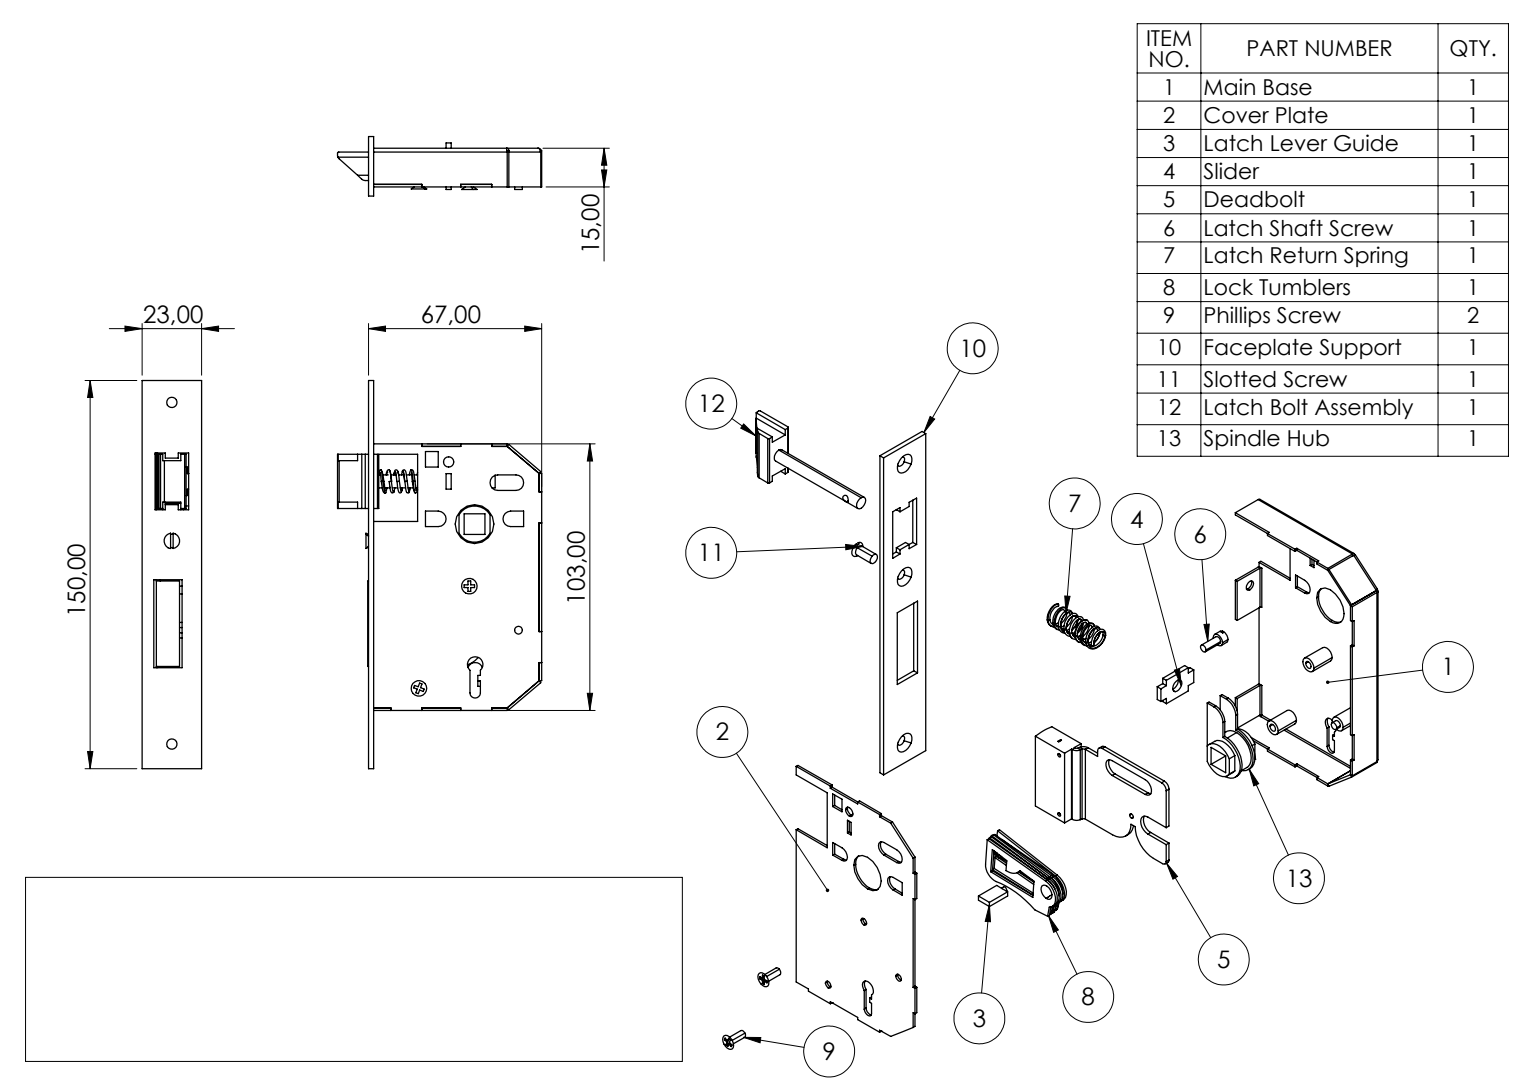
ISO-10303-21;
HEADER;
FILE_DESCRIPTION (('STEP AP214'),
    '1' );
FILE_NAME ('MAS-159',
    '2026-10-06T13:23:30',
    ( '' ),
    ( '' ),
    'SwSTEP 2.0',
    'SolidWorks 2020',
    '' );
FILE_SCHEMA (( 'AUTOMOTIVE_DESIGN' ));
ENDSEC;

DATA;
#1 = VERTEX_POINT ( 'NONE', #187 ) ;
#2 = FACE_OUTER_BOUND ( 'NONE', #19323, .T. ) ;
#3 = VECTOR ( 'NONE', #8048, 1000.000000000000000 ) ;
#4 = CARTESIAN_POINT ( 'NONE',  ( -30.49999999990000177, 47.50000000000000000, -147.5552959529999839 ) ) ;
#5 = CARTESIAN_POINT ( 'NONE',  ( -17.23399296970191941, 39.75881394383647915, -140.1956667236787553 ) ) ;
#6 = CARTESIAN_POINT ( 'NONE',  ( -31.50000000000000000, 10.25000000000000000, -137.0552959530000123 ) ) ;
#7 = ORIENTED_EDGE ( 'NONE', *, *, #14186, .F. ) ;
#8 = PLANE ( 'NONE',  #9401 ) ;
#9 = LINE ( 'NONE', #19761, #1381 ) ;
#10 = VECTOR ( 'NONE', #7060, 1000.000000000000000 ) ;
#11 = AXIS2_PLACEMENT_3D ( 'NONE', #8337, #8458, #15612 ) ;
#12 = LINE ( 'NONE', #7259, #31 ) ;
#13 = DIRECTION ( 'NONE',  ( 0.000000000000000000, 1.000000000000000000, 0.000000000000000000 ) ) ;
#14 = CARTESIAN_POINT ( 'NONE',  ( 7.750000000000000000, -40.23606797749999942, -150.0552959529999839 ) ) ;
#15 = VECTOR ( 'NONE', #22356, 1000.000000000000000 ) ;
#16 = CARTESIAN_POINT ( 'NONE',  ( -31.00000000000000000, 10.25000000000000000, -150.0552959529999839 ) ) ;
#17 = VECTOR ( 'NONE', #19861, 1000.000000000000114 ) ;
#18 = ORIENTED_EDGE ( 'NONE', *, *, #14112, .F. ) ;
#19 = EDGE_CURVE ( 'NONE', #10851, #14365, #21344, .T. ) ;
#20 = LINE ( 'NONE', #12366, #11445 ) ;
#21 = CARTESIAN_POINT ( 'NONE',  ( -13.53805010459570823, -42.60941606008491789, -136.0552959529695158 ) ) ;
#22 = EDGE_CURVE ( 'NONE', #8505, #15326, #21385, .T. ) ;
#23 = CARTESIAN_POINT ( 'NONE',  ( 6.899000527194547594, -5.343640159924734512, -150.0552959529999839 ) ) ;
#24 = CARTESIAN_POINT ( 'NONE',  ( -5.972224716186543603, 40.79464204718496489, -141.7656025440738006 ) ) ;
#25 = EDGE_CURVE ( 'NONE', #1116, #6470, #1636, .T. ) ;
#26 = CARTESIAN_POINT ( 'NONE',  ( 32.14594224149999491, 40.79958733410000349, -149.5552959519999945 ) ) ;
#27 = EDGE_LOOP ( 'NONE', ( #14113, #8328, #12180, #9090 ) ) ;
#28 = LINE ( 'NONE', #12848, #13253 ) ;
#29 = DIRECTION ( 'NONE',  ( -2.842170943040000002E-14, -3.552713678800000097E-13, -1.000000000000000000 ) ) ;
#30 = VERTEX_POINT ( 'NONE', #23278 ) ;
#31 = VECTOR ( 'NONE', #17982, 1000.000000000000000 ) ;
#32 = VECTOR ( 'NONE', #119, 1000.000000000000000 ) ;
#33 = DIRECTION ( 'NONE',  ( -2.257144641399999941E-12, 0.000000000000000000, -1.000000000000000000 ) ) ;
#34 = VERTEX_POINT ( 'NONE', #8858 ) ;
#35 = FACE_OUTER_BOUND ( 'NONE', #21489, .T. ) ;
#36 = CARTESIAN_POINT ( 'NONE',  ( -30.18072937777062492, 41.58839647259347316, -144.3146225325547505 ) ) ;
#37 = CARTESIAN_POINT ( 'NONE',  ( 5.631397321050000571, -17.85059010000000157, -146.5552959529999839 ) ) ;
#38 = CARTESIAN_POINT ( 'NONE',  ( 7.263251615191055777, 37.84880977052021223, -141.7037997430943790 ) ) ;
#39 = ORIENTED_EDGE ( 'NONE', *, *, #18140, .F. ) ;
#40 = CARTESIAN_POINT ( 'NONE',  ( -11.30159772195502299, 34.40649072814353815, -140.3533750429825773 ) ) ;
#41 = CARTESIAN_POINT ( 'NONE',  ( -19.36238656785138090, 32.32519816855536732, -144.8017779651653427 ) ) ;
#42 = DIRECTION ( 'NONE',  ( 0.000000000000000000, 1.000000000000000000, 0.000000000000000000 ) ) ;
#43 = DIRECTION ( 'NONE',  ( 0.000000000000000000, 1.000000000000000000, 0.000000000000000000 ) ) ;
#44 = ORIENTED_EDGE ( 'NONE', *, *, #15140, .T. ) ;
#45 = VECTOR ( 'NONE', #10247, 1000.000000000000000 ) ;
#46 = CARTESIAN_POINT ( 'NONE',  ( -26.35824191589999899, -34.50000000000000000, -150.0657682190000060 ) ) ;
#47 = ORIENTED_EDGE ( 'NONE', *, *, #19254, .F. ) ;
#48 = CARTESIAN_POINT ( 'NONE',  ( -8.100541861814468447, 36.99062475582145737, -140.7379126119401178 ) ) ;
#49 = DIRECTION ( 'NONE',  ( -2.507771768020000122E-12, -0.000000000000000000, 1.000000000000000000 ) ) ;
#50 = EDGE_CURVE ( 'NONE', #22537, #320, #23237, .T. ) ;
#51 = CARTESIAN_POINT ( 'NONE',  ( 23.00000000000000000, 25.50000000000000000, -151.0552959529999839 ) ) ;
#52 = ORIENTED_EDGE ( 'NONE', *, *, #9220, .T. ) ;
#53 = DIRECTION ( 'NONE',  ( 1.000000000000000000, 0.000000000000000000, 0.000000000000000000 ) ) ;
#54 = LINE ( 'NONE', #14445, #10 ) ;
#55 = ORIENTED_EDGE ( 'NONE', *, *, #18140, .T. ) ;
#56 = CARTESIAN_POINT ( 'NONE',  ( -17.71126569040000120, 40.30718541979999969, -145.9389846960000057 ) ) ;
#57 = EDGE_CURVE ( 'NONE', #16606, #2360, #10514, .T. ) ;
#58 = CARTESIAN_POINT ( 'NONE',  ( 18.66060904160396916, 20.09818317339116689, -150.0552959529999839 ) ) ;
#59 = CARTESIAN_POINT ( 'NONE',  ( -15.75723547076485254, -44.30951848884578226, -150.0552959529999839 ) ) ;
#60 = AXIS2_PLACEMENT_3D ( 'NONE', #23173, #12444, #1408 ) ;
#61 = CLOSED_SHELL ( 'NONE', ( #2527, #3162, #21913, #12259, #23509, #6478, #21323, #18404, #11266, #1129, #5411, #9358, #21072, #12421, #16618, #19421, #14593, #11107, #12865, #16221, #14697, #10087, #8870, #20532, #21101, #11720, #17202, #7335, #11973, #7291, #21318, #13553, #10889, #7699, #12447, #10834 ) ) ;
#62 = FACE_OUTER_BOUND ( 'NONE', #19920, .T. ) ;
#63 = VECTOR ( 'NONE', #17679, 1000.000000000000000 ) ;
#64 = LINE ( 'NONE', #5521, #16191 ) ;
#65 = LINE ( 'NONE', #14804, #22679 ) ;
#66 = PLANE ( 'NONE',  #21173 ) ;
#67 = CARTESIAN_POINT ( 'NONE',  ( 15.97954986339999905, -26.72957102550000030, -142.5552959529999839 ) ) ;
#68 = EDGE_CURVE ( 'NONE', #3612, #21024, #1516, .T. ) ;
#69 = CARTESIAN_POINT ( 'NONE',  ( -4.946601369560000627, -23.77962690289999870, -143.5552959529999839 ) ) ;
#70 = VERTEX_POINT ( 'NONE', #16012 ) ;
#71 = ORIENTED_EDGE ( 'NONE', *, *, #16428, .T. ) ;
#72 =( NAMED_UNIT ( * ) PLANE_ANGLE_UNIT ( ) SI_UNIT ( $, .RADIAN. ) );
#73 = VERTEX_POINT ( 'NONE', #5299 ) ;
#74 = FACE_OUTER_BOUND ( 'NONE', #19510, .T. ) ;
#75 = CARTESIAN_POINT ( 'NONE',  ( 7.750000000000000000, -40.23606797749999942, -150.5552959529999839 ) ) ;
#76 = VERTEX_POINT ( 'NONE', #12547 ) ;
#77 = AXIS2_PLACEMENT_3D ( 'NONE', #19282, #2992, #15716 ) ;
#78 = EDGE_CURVE ( 'NONE', #537, #6609, #18037, .T. ) ;
#79 = CIRCLE ( 'NONE', #13356, 2.000000000000000000 ) ;
#80 = CARTESIAN_POINT ( 'NONE',  ( 1.600095057559999923, -18.40127899619999852, -146.5552959529999839 ) ) ;
#81 = VECTOR ( 'NONE', #14435, 1000.000000000000114 ) ;
#82 = ORIENTED_EDGE ( 'NONE', *, *, #12596, .T. ) ;
#83 = CARTESIAN_POINT ( 'NONE',  ( 6.499999999879999102, -3.000000000000000000, -135.2552959529999725 ) ) ;
#84 = CARTESIAN_POINT ( 'NONE',  ( -19.91646121121569735, 34.85517757522313076, -141.3256718703773629 ) ) ;
#85 = CARTESIAN_POINT ( 'NONE',  ( -30.02199999990000023, 40.03108891319999429, -145.8052959529999839 ) ) ;
#86 = CARTESIAN_POINT ( 'NONE',  ( 15.50000000000000000, 39.50000000000000000, -136.0552959530000123 ) ) ;
#87 = ORIENTED_EDGE ( 'NONE', *, *, #14036, .T. ) ;
#88 = DIRECTION ( 'NONE',  ( 2.257749542879999954E-12, 0.000000000000000000, 1.000000000000000000 ) ) ;
#89 = ORIENTED_EDGE ( 'NONE', *, *, #22160, .F. ) ;
#90 = EDGE_CURVE ( 'NONE', #4045, #3279, #299, .T. ) ;
#91 = CARTESIAN_POINT ( 'NONE',  ( 9.327001754561790037, 35.74856537270147783, -141.8910607813375009 ) ) ;
#92 = DIRECTION ( 'NONE',  ( -2.257144641399999941E-12, 8.049635416090000264E-35, -1.000000000000000000 ) ) ;
#93 = DIRECTION ( 'NONE',  ( -0.9892101392001054760, 0.1465035852930155480, 4.471739159800472250E-12 ) ) ;
#94 = VECTOR ( 'NONE', #6253, 1000.000000000000000 ) ;
#95 = ORIENTED_EDGE ( 'NONE', *, *, #4265, .F. ) ;
#96 = VECTOR ( 'NONE', #17767, 1000.000000000000227 ) ;
#97 = AXIS2_PLACEMENT_3D ( 'NONE', #8071, #2741, #23074 ) ;
#98 = EDGE_CURVE ( 'NONE', #6545, #18690, #5646, .T. ) ;
#99 = EDGE_CURVE ( 'NONE', #3836, #1507, #11570, .T. ) ;
#100 = PLANE ( 'NONE',  #11800 ) ;
#101 = ORIENTED_EDGE ( 'NONE', *, *, #18336, .T. ) ;
#102 = DIRECTION ( 'NONE',  ( 0.000000000000000000, -1.000000000000000000, 0.000000000000000000 ) ) ;
#103 = CARTESIAN_POINT ( 'NONE',  ( -6.024730888589999722, -51.50000000000000000, -149.5552959529999839 ) ) ;
#104 = EDGE_CURVE ( 'NONE', #6667, #13256, #16589, .T. ) ;
#105 = ORIENTED_EDGE ( 'NONE', *, *, #1127, .F. ) ;
#106 = PLANE ( 'NONE',  #15659 ) ;
#107 = ORIENTED_EDGE ( 'NONE', *, *, #17048, .F. ) ;
#108 = CARTESIAN_POINT ( 'NONE',  ( -21.95493828276233472, 34.13232134794248651, -147.9325040407576353 ) ) ;
#109 = EDGE_CURVE ( 'NONE', #2866, #16847, #2210, .T. ) ;
#110 = CARTESIAN_POINT ( 'NONE',  ( -25.86630785129999666, -51.50000000000000000, -136.5552959530000123 ) ) ;
#111 = ORIENTED_EDGE ( 'NONE', *, *, #15327, .F. ) ;
#112 = APPLICATION_PROTOCOL_DEFINITION ( 'draft international standard', 'automotive_design', 1998, #2963 ) ;
#113 = ORIENTED_EDGE ( 'NONE', *, *, #15897, .T. ) ;
#114 = CARTESIAN_POINT ( 'NONE',  ( -26.86882954950000268, 40.29793777999999804, -142.0811670120000088 ) ) ;
#115 = FACE_OUTER_BOUND ( 'NONE', #19032, .T. ) ;
#116 = MECHANICAL_DESIGN_GEOMETRIC_PRESENTATION_REPRESENTATION (  '', ( #11103 ), #3517 ) ;
#117 = CARTESIAN_POINT ( 'NONE',  ( -4.959431410700000598, -23.66636161550000139, -146.0552959529999839 ) ) ;
#118 = AXIS2_PLACEMENT_3D ( 'NONE', #14379, #10436, #6880 ) ;
#119 = DIRECTION ( 'NONE',  ( -1.000000000000000000, 0.000000000000000000, 2.245315044999999693E-12 ) ) ;
#120 = LINE ( 'NONE', #16055, #20099 ) ;
#121 = ORIENTED_EDGE ( 'NONE', *, *, #3001, .T. ) ;
#122 = CARTESIAN_POINT ( 'NONE',  ( -4.160432423080000497, -28.71743394529999804, -144.5552959529999839 ) ) ;
#123 = CARTESIAN_POINT ( 'NONE',  ( 10.38320006080000013, -24.50000000000000000, -148.5552959529999839 ) ) ;
#124 = ORIENTED_EDGE ( 'NONE', *, *, #13380, .T. ) ;
#125 = LINE ( 'NONE', #11042, #20030 ) ;
#126 = DIRECTION ( 'NONE',  ( 0.000000000000000000, 0.000000000000000000, 1.000000000000000000 ) ) ;
#127 = EDGE_CURVE ( 'NONE', #16762, #17721, #6116, .T. ) ;
#128 = CARTESIAN_POINT ( 'NONE',  ( -17.11288009319332915, 40.89466944836319584, -143.6359263498834196 ) ) ;
#129 = DIRECTION ( 'NONE',  ( -0.9896415801065050477, 0.1435602414469278887, 8.992806499463764746E-12 ) ) ;
#130 = EDGE_LOOP ( 'NONE', ( #1409, #6613, #421, #6495 ) ) ;
#131 = FACE_OUTER_BOUND ( 'NONE', #19542, .T. ) ;
#132 = DIRECTION ( 'NONE',  ( 1.000000000000000000, 0.000000000000000000, 0.000000000000000000 ) ) ;
#133 = CARTESIAN_POINT ( 'NONE',  ( 5.631397321050000571, -17.85059010000000157, -146.5552959529999839 ) ) ;
#134 = LINE ( 'NONE', #14635, #4183 ) ;
#135 = DIRECTION ( 'NONE',  ( 1.000000000000000000, 2.602084704489999637E-17, 0.000000000000000000 ) ) ;
#136 = LINE ( 'NONE', #21434, #17431 ) ;
#137 = ORIENTED_EDGE ( 'NONE', *, *, #3234, .F. ) ;
#138 = DIRECTION ( 'NONE',  ( 1.000000000000000000, 0.000000000000000000, -2.257560236040000027E-12 ) ) ;
#139 = CARTESIAN_POINT ( 'NONE',  ( -26.35824191589999899, -34.50000000000000000, -141.0657682190000060 ) ) ;
#140 = CARTESIAN_POINT ( 'NONE',  ( -18.07392865170000107, -1.500000000000000000, -147.3157682190000060 ) ) ;
#141 = CARTESIAN_POINT ( 'NONE',  ( -7.010349702009219364, 37.05829245175948472, -148.1453878979395995 ) ) ;
#142 = CARTESIAN_POINT ( 'NONE',  ( -13.80049973640272931, -43.92182007996237303, -136.0552959530027124 ) ) ;
#143 = EDGE_LOOP ( 'NONE', ( #7087, #11554, #3660, #16017 ) ) ;
#144 = CARTESIAN_POINT ( 'NONE',  ( 9.683200060759999062, -20.50000000000000000, -149.3052959529999839 ) ) ;
#145 = FACE_BOUND ( 'NONE', #10019, .T. ) ;
#146 = AXIS2_PLACEMENT_3D ( 'NONE', #6998, #10782, #18066 ) ;
#147 = ORIENTED_EDGE ( 'NONE', *, *, #18826, .F. ) ;
#148 = ORIENTED_EDGE ( 'NONE', *, *, #4162, .F. ) ;
#149 = CARTESIAN_POINT ( 'NONE',  ( 5.420128080818026106, -2.298969449354696604, -136.0552959530122337 ) ) ;
#150 = EDGE_CURVE ( 'NONE', #19192, #2146, #2095, .T. ) ;
#151 = CARTESIAN_POINT ( 'NONE',  ( -29.72253042784264210, 40.43424528537140361, -140.6915255650335723 ) ) ;
#152 = PLANE ( 'NONE',  #286 ) ;
#153 = CARTESIAN_POINT ( 'NONE',  ( 8.154916571317706087, 35.54018629028437459, -142.0257885890718512 ) ) ;
#154 = VERTEX_POINT ( 'NONE', #4337 ) ;
#155 = CARTESIAN_POINT ( 'NONE',  ( -10.36638211085415584, 32.95473824138212393, -141.4495653476137704 ) ) ;
#156 = CARTESIAN_POINT ( 'NONE',  ( -18.21358191688009498, 34.41669922854067920, -147.7040578527177388 ) ) ;
#157 = DIRECTION ( 'NONE',  ( 0.000000000000000000, 1.000000000000000000, 0.000000000000000000 ) ) ;
#158 = CARTESIAN_POINT ( 'NONE',  ( 9.295843182404178506, -32.13416640351051967, -136.0552959530209876 ) ) ;
#159 = CARTESIAN_POINT ( 'NONE',  ( -22.66750349916592810, 37.99877533998466816, -139.6205617058595294 ) ) ;
#160 = LINE ( 'NONE', #11080, #6868 ) ;
#161 = AXIS2_PLACEMENT_3D ( 'NONE', #17240, #17123, #840 ) ;
#162 = FACE_OUTER_BOUND ( 'NONE', #18152, .T. ) ;
#163 = DIRECTION ( 'NONE',  ( -2.808280234689999718E-18, 1.000000000000000000, 1.592654863519999645E-17 ) ) ;
#164 = CARTESIAN_POINT ( 'NONE',  ( -9.056357402059999728, -12.43025388040000045, -147.5552959529999839 ) ) ;
#165 = ORIENTED_EDGE ( 'NONE', *, *, #16079, .F. ) ;
#166 = CARTESIAN_POINT ( 'NONE',  ( -5.932764524189999555, 37.76833845600000217, -147.9772051180000005 ) ) ;
#167 = EDGE_LOOP ( 'NONE', ( #4339, #16056, #21520, #10157 ) ) ;
#168 = LINE ( 'NONE', #11551, #791 ) ;
#169 = CARTESIAN_POINT ( 'NONE',  ( 32.50000000000000000, 40.03620104880000241, -143.0552959529999839 ) ) ;
#170 = DIRECTION ( 'NONE',  ( -0.7071067811865474617, -0.7071067811865476838, 0.000000000000000000 ) ) ;
#171 = CARTESIAN_POINT ( 'NONE',  ( -3.500000000000000000, 44.50000000000000000, -150.0552959529999839 ) ) ;
#172 = ADVANCED_FACE ( 'NONE', ( #21960 ), #4222, .F. ) ;
#173 = DIRECTION ( 'NONE',  ( -0.09606172499277214338, -0.9953753789357123738, 8.234154099303244678E-13 ) ) ;
#174 = VECTOR ( 'NONE', #17768, 1000.000000000000000 ) ;
#175 = CARTESIAN_POINT ( 'NONE',  ( -7.816799939239999162, -1.500000000000000000, -148.5552959529999839 ) ) ;
#176 = DIRECTION ( 'NONE',  ( 2.507771768019999718E-12, 1.592654864069999939E-17, -1.000000000000000000 ) ) ;
#177 = EDGE_CURVE ( 'NONE', #22553, #21627, #7661, .T. ) ;
#178 = CARTESIAN_POINT ( 'NONE',  ( -1.499999999960000219, 44.50000000000000000, -136.0552959530000123 ) ) ;
#179 = PRODUCT ( 'Latch Shaft Screw', 'Latch Shaft Screw', '', ( #7074 ) ) ;
#180 = CARTESIAN_POINT ( 'NONE',  ( -33.42928932190000069, 66.02782287919998794, -146.7500980969999773 ) ) ;
#181 = ORIENTED_EDGE ( 'NONE', *, *, #506, .F. ) ;
#182 = UNCERTAINTY_MEASURE_WITH_UNIT (LENGTH_MEASURE( 1.000000000000000082E-05 ), #19737, 'distance_accuracy_value', 'NONE');
#183 = EDGE_LOOP ( 'NONE', ( #12514, #3187, #13299, #6261 ) ) ;
#184 = EDGE_LOOP ( 'NONE', ( #18556, #23230 ) ) ;
#185 = CARTESIAN_POINT ( 'NONE',  ( -16.74070468267852618, 33.96681352825373779, -142.1712902011884978 ) ) ;
#186 = CARTESIAN_POINT ( 'NONE',  ( 31.50000000000000000, 39.80430157320000006, -149.5552959529999839 ) ) ;
#187 = CARTESIAN_POINT ( 'NONE',  ( -20.60824191591068555, -32.00000000000000000, -141.9623572383543717 ) ) ;
#188 = CARTESIAN_POINT ( 'NONE',  ( 31.00000000000000000, 39.80430157320000006, -150.0552959529999839 ) ) ;
#189 = ORIENTED_EDGE ( 'NONE', *, *, #7703, .T. ) ;
#190 = DIRECTION ( 'NONE',  ( -2.257039000139999987E-12, 0.000000000000000000, -1.000000000000000000 ) ) ;
#191 = CARTESIAN_POINT ( 'NONE',  ( -19.09494877074376262, 33.54410563133428269, -142.1858765932176141 ) ) ;
#192 = CARTESIAN_POINT ( 'NONE',  ( 31.50000000000000000, 36.50000000000000000, -137.0552959530000123 ) ) ;
#193 = ORIENTED_EDGE ( 'NONE', *, *, #5602, .T. ) ;
#194 = LINE ( 'NONE', #5434, #7982 ) ;
#195 = EDGE_CURVE ( 'NONE', #7827, #16530, #20002, .T. ) ;
#196 = CARTESIAN_POINT ( 'NONE',  ( -31.00000000000000000, -50.00000000000000000, -151.0552959529999839 ) ) ;
#197 = CARTESIAN_POINT ( 'NONE',  ( -14.47770030809999930, -1.500000000000000000, -149.3052959529999839 ) ) ;
#198 = CARTESIAN_POINT ( 'NONE',  ( 15.50000000000000000, 36.50000000000000000, -151.0552959529999839 ) ) ;
#199 = EDGE_CURVE ( 'NONE', #11395, #18017, #9780, .T. ) ;
#200 = ORIENTED_EDGE ( 'NONE', *, *, #6768, .F. ) ;
#201 = FACE_BOUND ( 'NONE', #2736, .T. ) ;
#202 = ORIENTED_EDGE ( 'NONE', *, *, #2694, .F. ) ;
#203 = VECTOR ( 'NONE', #22611, 1000.000000000000000 ) ;
#204 = CARTESIAN_POINT ( 'NONE',  ( 5.523675324909882001, -48.60111558252668829, -150.0552959529999839 ) ) ;
#205 = ORIENTED_EDGE ( 'NONE', *, *, #17674, .T. ) ;
#206 = CARTESIAN_POINT ( 'NONE',  ( -26.46126365530976443, 39.05410761395327057, -141.1838645948565443 ) ) ;
#207 = ORIENTED_EDGE ( 'NONE', *, *, #948, .T. ) ;
#208 = CARTESIAN_POINT ( 'NONE',  ( -23.51619327739999932, 36.94101002280000046, -140.1031831869999849 ) ) ;
#210 = ADVANCED_FACE ( 'NONE', ( #13249 ), #13024, .F. ) ;
#209 = STYLED_ITEM ( 'NONE', ( #19357 ), #4113 ) ;
#211 = EDGE_LOOP ( 'NONE', ( #21021, #20847, #5085, #22198, #20574, #16740, #10421 ) ) ;
#212 = CARTESIAN_POINT ( 'NONE',  ( -17.62135916506277411, -44.51085694111269930, -150.0552959529999555 ) ) ;
#213 = VERTEX_POINT ( 'NONE', #20525 ) ;
#214 = CARTESIAN_POINT ( 'NONE',  ( 0.000000000000000000, 0.000000000000000000, 0.000000000000000000 ) ) ;
#215 = ORIENTED_EDGE ( 'NONE', *, *, #20592, .F. ) ;
#216 = CARTESIAN_POINT ( 'NONE',  ( -4.499999999959999109, 34.00000000000000000, -153.0552959529999839 ) ) ;
#217 =( REPRESENTATION_RELATIONSHIP ('NONE','NONE', #7672, #13440 ) REPRESENTATION_RELATIONSHIP_WITH_TRANSFORMATION ( #16002 )SHAPE_REPRESENTATION_RELATIONSHIP( ) );
#218 = LINE ( 'NONE', #15834, #14813 ) ;
#219 = CARTESIAN_POINT ( 'NONE',  ( -13.86630785130000021, 51.50000000000000000, -136.5552959530000123 ) ) ;
#220 = CARTESIAN_POINT ( 'NONE',  ( -16.93971969060000049, -1.500000000000000000, -147.9894163970000136 ) ) ;
#221 = CARTESIAN_POINT ( 'NONE',  ( -11.29029698198118048, 36.23043332044583309, -140.4049246345721826 ) ) ;
#222 = ADVANCED_FACE ( 'NONE', ( #11458 ), #4098, .F. ) ;
#223 = CARTESIAN_POINT ( 'NONE',  ( -9.052249647940781685, 41.71831906193862949, -143.4732298663905965 ) ) ;
#224 = ORIENTED_EDGE ( 'NONE', *, *, #1037, .F. ) ;
#225 = EDGE_CURVE ( 'NONE', #11906, #13032, #16136, .T. ) ;
#226 = DIRECTION ( 'NONE',  ( 0.000000000000000000, 1.000000000000000000, 0.000000000000000000 ) ) ;
#227 = VECTOR ( 'NONE', #9869, 1000.000000000000000 ) ;
#228 = VECTOR ( 'NONE', #3998, 1000.000000000000000 ) ;
#229 = EDGE_CURVE ( 'NONE', #213, #5505, #1240, .T. ) ;
#230 = CARTESIAN_POINT ( 'NONE',  ( 9.034463386642046956, 35.59814294577384430, -146.1252975212060505 ) ) ;
#231 = EDGE_CURVE ( 'NONE', #11233, #3677, #3985, .T. ) ;
#232 = VERTEX_POINT ( 'NONE', #4927 ) ;
#233 = CARTESIAN_POINT ( 'NONE',  ( -6.601136089949999786, -20.10368962670000315, -144.5552959529999839 ) ) ;
#234 = CARTESIAN_POINT ( 'NONE',  ( 3.611688725869999975E-11, 34.00000000000000000, -136.0552959530000123 ) ) ;
#235 = CARTESIAN_POINT ( 'NONE',  ( -17.12614424251881573, 38.90004930153931895, -139.7093083313472448 ) ) ;
#236 = CARTESIAN_POINT ( 'NONE',  ( -29.46750132911070352, 41.44936499793962525, -145.0977680319627439 ) ) ;
#237 = ORIENTED_EDGE ( 'NONE', *, *, #19571, .F. ) ;
#238 = CARTESIAN_POINT ( 'NONE',  ( -7.816799939239999162, -0.2500000000010000334, -150.0552959529999839 ) ) ;
#239 = CARTESIAN_POINT ( 'NONE',  ( 32.50000000000000000, 0.000000000000000000, -136.0552959530000123 ) ) ;
#240 = DIRECTION ( 'NONE',  ( 0.000000000000000000, 0.000000000000000000, 1.000000000000000000 ) ) ;
#241 = CARTESIAN_POINT ( 'NONE',  ( -7.047250123649999587, -34.50000000000000000, -148.5552959529999839 ) ) ;
#242 = CARTESIAN_POINT ( 'NONE',  ( -18.09080689940000397, 41.54765954780000214, -144.4256796519999853 ) ) ;
#243 = CARTESIAN_POINT ( 'NONE',  ( -9.347107914279998653, -17.32706600430000066, -144.5552959529999839 ) ) ;
#244 = B_SPLINE_CURVE_WITH_KNOTS ( 'NONE', 3,
 ( #8410, #6271, #1182, #22691, #19238, #11612, #9949, #19010, #11855, #8520, #3074, #13524, #13649, #10184, #20796, #15682, #4613, #4491 ),
 .UNSPECIFIED., .F., .F.,
 ( 4, 2, 2, 2, 2, 2, 2, 2, 4 ),
 ( 0.000000000000000000, 0.1250000000000000000, 0.2500000000000000000, 0.3750000000000000000, 0.5000000000000000000, 0.6250000000000000000, 0.7500000000000000000, 0.8750000000000000000, 1.000000000000000000 ),
 .UNSPECIFIED. ) ;
#245 = VECTOR ( 'NONE', #2038, 1000.000000000000114 ) ;
#246 = VECTOR ( 'NONE', #23462, 1000.000000000000000 ) ;
#247 = ORIENTED_EDGE ( 'NONE', *, *, #12729, .T. ) ;
#248 =( NAMED_UNIT ( * ) SI_UNIT ( $, .STERADIAN. ) SOLID_ANGLE_UNIT ( ) );
#249 = LINE ( 'NONE', #5710, #16739 ) ;
#250 = CARTESIAN_POINT ( 'NONE',  ( 4.107300918301284298, -6.500000000000002665, -150.0552959529999839 ) ) ;
#251 = CARTESIAN_POINT ( 'NONE',  ( 10.50000000010000001, 20.50000000000000000, -150.5552959529999839 ) ) ;
#252 = CARTESIAN_POINT ( 'NONE',  ( -10.92854443050000057, 33.70908472050000171, -142.0058283510000194 ) ) ;
#253 = EDGE_LOOP ( 'NONE', ( #22438, #23060, #147, #8100 ) ) ;
#254 = EDGE_CURVE ( 'NONE', #1659, #23125, #22884, .T. ) ;
#255 = CARTESIAN_POINT ( 'NONE',  ( -27.13199227600000185, 40.71900643419999710, -144.3906906950000177 ) ) ;
#256 = ADVANCED_FACE ( 'NONE', ( #12174 ), #12050, .F. ) ;
#257 = LINE ( 'NONE', #7499, #9038 ) ;
#258 = VERTEX_POINT ( 'NONE', #1012 ) ;
#259 = VECTOR ( 'NONE', #18453, 1000.000000000000114 ) ;
#260 = ORIENTED_EDGE ( 'NONE', *, *, #13143, .F. ) ;
#261 = CARTESIAN_POINT ( 'NONE',  ( -35.47299999999999898, 14.00000000000000000, -143.5552959529999839 ) ) ;
#262 = DIRECTION ( 'NONE',  ( 0.000000000000000000, 1.000000000000000000, 0.000000000000000000 ) ) ;
#263 = CARTESIAN_POINT ( 'NONE',  ( -9.923478264230000789, -23.29931827799999766, -144.5552959529999839 ) ) ;
#264 = ORIENTED_EDGE ( 'NONE', *, *, #15241, .F. ) ;
#265 = PLANE ( 'NONE',  #18891 ) ;
#266 = CARTESIAN_POINT ( 'NONE',  ( -19.59255166828732087, 37.05126161859348599, -140.3061871182880225 ) ) ;
#267 = CARTESIAN_POINT ( 'NONE',  ( -4.499999999949999996, 40.00000000000000000, -150.0552959529999839 ) ) ;
#268 = CARTESIAN_POINT ( 'NONE',  ( 12.88103053862586478, 34.98519100497017575, -136.0552959530290593 ) ) ;
#269 = CARTESIAN_POINT ( 'NONE',  ( -22.77297780190586707, 38.93970885093763457, -139.8786318329592291 ) ) ;
#270 = CARTESIAN_POINT ( 'NONE',  ( 9.683200060760000838, -20.36785913719859664, -148.5552959529999839 ) ) ;
#271 = CIRCLE ( 'NONE', #1413, 2.000000000000001776 ) ;
#272 = VECTOR ( 'NONE', #12599, 1000.000000000000227 ) ;
#273 = DIRECTION ( 'NONE',  ( -1.000000000000000000, -3.994014902950000436E-29, 0.000000000000000000 ) ) ;
#274 = CARTESIAN_POINT ( 'NONE',  ( 7.750000000030000002, -37.98606797749999942, -136.5552959530000123 ) ) ;
#275 = FACE_OUTER_BOUND ( 'NONE', #1405, .T. ) ;
#276 = ORIENTED_EDGE ( 'NONE', *, *, #19287, .F. ) ;
#277 = EDGE_CURVE ( 'NONE', #1162, #21810, #7303, .T. ) ;
#278 = CARTESIAN_POINT ( 'NONE',  ( 8.750000000000000000, -42.23606797749999942, -150.5552959529999839 ) ) ;
#279 = EDGE_CURVE ( 'NONE', #18237, #3022, #18705, .T. ) ;
#280 = ORIENTED_EDGE ( 'NONE', *, *, #14964, .T. ) ;
#281 = CARTESIAN_POINT ( 'NONE',  ( -15.50000000000000000, 34.50000000000000000, -151.0552959529999839 ) ) ;
#282 = DIRECTION ( 'NONE',  ( 0.000000000000000000, -1.000000000000000000, 0.000000000000000000 ) ) ;
#283 = DIRECTION ( 'NONE',  ( 2.602084747549999882E-17, -1.000000000000000000, -5.873289694040000105E-29 ) ) ;
#284 = FACE_OUTER_BOUND ( 'NONE', #6510, .T. ) ;
#285 = CARTESIAN_POINT ( 'NONE',  ( -13.05114220192597507, 34.48316525647341990, -140.6280605682619864 ) ) ;
#286 = AXIS2_PLACEMENT_3D ( 'NONE', #3950, #12631, #10950 ) ;
#287 = CARTESIAN_POINT ( 'NONE',  ( -9.969904307360000217, -22.67446893780000039, -144.5552959529999839 ) ) ;
#288 = AXIS2_PLACEMENT_3D ( 'NONE', #20395, #13474, #22534 ) ;
#289 = CARTESIAN_POINT ( 'NONE',  ( 14.71905350739799623, 33.57650987475365412, -150.0552959530000123 ) ) ;
#290 = CONTEXT_DEPENDENT_SHAPE_REPRESENTATION ( #7944, #22651 ) ;
#291 = CARTESIAN_POINT ( 'NONE',  ( -0.7499999998410000757, 41.50000000000000000, -139.5552959529999839 ) ) ;
#292 = LINE ( 'NONE', #7531, #4006 ) ;
#293 = CARTESIAN_POINT ( 'NONE',  ( -16.50000000000000000, -43.00000000000000000, -136.0552959530000123 ) ) ;
#294 = ORIENTED_EDGE ( 'NONE', *, *, #9256, .T. ) ;
#295 = ORIENTED_EDGE ( 'NONE', *, *, #21236, .T. ) ;
#296 = SHAPE_REPRESENTATION_RELATIONSHIP ( 'NONE' , 'NONE' ,  #13440, #10650 ) ;
#297 = ORIENTED_EDGE ( 'NONE', *, *, #254, .T. ) ;
#298 = DIRECTION ( 'NONE',  ( 1.000000000000000000, 0.000000000000000000, 0.000000000000000000 ) ) ;
#299 = LINE ( 'NONE', #2335, #3484 ) ;
#300 = LINE ( 'NONE', #16373, #22571 ) ;
#301 = VECTOR ( 'NONE', #7137, 1000.000000000000000 ) ;
#302 = EDGE_LOOP ( 'NONE', ( #10238, #8735, #12930, #17915, #645, #16858 ) ) ;
#303 = EDGE_CURVE ( 'NONE', #11439, #22823, #3876, .T. ) ;
#304 = LINE ( 'NONE', #18742, #12898 ) ;
#305 = CARTESIAN_POINT ( 'NONE',  ( 3.611688725869999975E-11, -37.98606797749999942, -136.0552959530000123 ) ) ;
#306 = STYLED_ITEM ( 'NONE', ( #22127 ), #19901 ) ;
#307 = EDGE_CURVE ( 'NONE', #18180, #4474, #17692, .T. ) ;
#308 = DIRECTION ( 'NONE',  ( 2.257144641397284947E-12, 2.714724913984255017E-24, 1.000000000000000000 ) ) ;
#309 = EDGE_LOOP ( 'NONE', ( #20160, #3924, #21001, #22212 ) ) ;
#310 = CARTESIAN_POINT ( 'NONE',  ( -20.84115054893410601, 39.15569877547226696, -141.0545280455379782 ) ) ;
#311 = CARTESIAN_POINT ( 'NONE',  ( 9.886079879350434751, 37.57350691547503629, -141.6219378633946917 ) ) ;
#312 = DIRECTION ( 'NONE',  ( 2.257144641399999941E-12, -4.009147065140000298E-51, 1.000000000000000000 ) ) ;
#313 = PLANE ( 'NONE',  #6728 ) ;
#314 = ORIENTED_EDGE ( 'NONE', *, *, #22, .F. ) ;
#315 = AXIS2_PLACEMENT_3D ( 'NONE', #12975, #16085, #23342 ) ;
#316 = FACE_OUTER_BOUND ( 'NONE', #21887, .T. ) ;
#317 = CONICAL_SURFACE ( 'NONE', #15128, 1.999999999999992450, 0.7853981633970000820 ) ;
#318 = ORIENTED_EDGE ( 'NONE', *, *, #17684, .T. ) ;
#319 = CARTESIAN_POINT ( 'NONE',  ( 6.229273316114841919, -48.94892946173367676, -150.0552959529999839 ) ) ;
#320 = VERTEX_POINT ( 'NONE', #3034 ) ;
#321 = CARTESIAN_POINT ( 'NONE',  ( -26.41333858494015630, 40.49754993825023064, -143.6922548833833559 ) ) ;
#322 = VERTEX_POINT ( 'NONE', #6472 ) ;
#323 = FACE_OUTER_BOUND ( 'NONE', #460, .T. ) ;
#324 = ORIENTED_EDGE ( 'NONE', *, *, #8627, .T. ) ;
#325 = CARTESIAN_POINT ( 'NONE',  ( -9.434278515689999978, -18.41834002140000237, -147.5552959529999839 ) ) ;
#326 = ORIENTED_EDGE ( 'NONE', *, *, #7122, .T. ) ;
#327 = DIRECTION ( 'NONE',  ( 0.000000000000000000, 0.000000000000000000, 1.000000000000000000 ) ) ;
#328 = VERTEX_POINT ( 'NONE', #17655 ) ;
#329 = CARTESIAN_POINT ( 'NONE',  ( -29.13601448249999848, 36.98639052360000079, -140.5419328609999923 ) ) ;
#330 = CARTESIAN_POINT ( 'NONE',  ( -23.51619327739999932, 36.94101002280000046, -140.1031831869999849 ) ) ;
#331 = CARTESIAN_POINT ( 'NONE',  ( 13.76008370043819973, 22.44588062467436629, -150.0552959529999839 ) ) ;
#332 = ADVANCED_FACE ( 'NONE', ( #22541 ), #3148, .T. ) ;
#333 = LINE ( 'NONE', #16862, #716 ) ;
#334 = FACE_OUTER_BOUND ( 'NONE', #6848, .T. ) ;
#335 = AXIS2_PLACEMENT_3D ( 'NONE', #20333, #9473, #5804 ) ;
#336 = PLANE ( 'NONE',  #4892 ) ;
#337 = ORIENTED_EDGE ( 'NONE', *, *, #14672, .T. ) ;
#338 = AXIS2_PLACEMENT_3D ( 'NONE', #22132, #13076, #20347 ) ;
#339 = CARTESIAN_POINT ( 'NONE',  ( 22.50000000000000000, 33.50000000000000000, -137.0552959530000123 ) ) ;
#340 = VECTOR ( 'NONE', #23038, 1000.000000000000000 ) ;
#341 = PRODUCT_RELATED_PRODUCT_CATEGORY ( 'part', '', ( #21568 ) ) ;
#342 = DIRECTION ( 'NONE',  ( 0.02818224575639410520, 0.9996028016287901163, -8.199401781418279957E-13 ) ) ;
#343 = VECTOR ( 'NONE', #12000, 1000.000000000000000 ) ;
#344 = EDGE_CURVE ( 'NONE', #6561, #14370, #10508, .T. ) ;
#345 = ORIENTED_EDGE ( 'NONE', *, *, #18029, .T. ) ;
#346 = DIRECTION ( 'NONE',  ( 2.257171095940000041E-12, 1.003664318210000046E-28, 1.000000000000000000 ) ) ;
#347 = CARTESIAN_POINT ( 'NONE',  ( -12.26329284728311997, 39.72411301547229101, -147.9408354451884122 ) ) ;
#348 = CARTESIAN_POINT ( 'NONE',  ( -16.81794493329665841, 37.02435727937783838, -140.5111119823167769 ) ) ;
#349 = CARTESIAN_POINT ( 'NONE',  ( -29.33124862419971635, 40.50047896906287548, -145.5019065615213663 ) ) ;
#350 = VERTEX_POINT ( 'NONE', #15287 ) ;
#351 = DIRECTION ( 'NONE',  ( 0.000000000000000000, -1.000000000000000000, 0.000000000000000000 ) ) ;
#352 = FACE_OUTER_BOUND ( 'NONE', #5067, .T. ) ;
#353 = AXIS2_PLACEMENT_3D ( 'NONE', #12297, #17774, #23258 ) ;
#354 = EDGE_CURVE ( 'NONE', #22442, #21113, #20876, .T. ) ;
#355 = ORIENTED_EDGE ( 'NONE', *, *, #21836, .T. ) ;
#356 = CARTESIAN_POINT ( 'NONE',  ( -8.296392858609999976, -9.821782169089999570, -148.5552959529999839 ) ) ;
#357 = FACE_OUTER_BOUND ( 'NONE', #9688, .T. ) ;
#358 = LINE ( 'NONE', #7600, #2620 ) ;
#359 = VECTOR ( 'NONE', #21287, 1000.000000000000000 ) ;
#360 = CARTESIAN_POINT ( 'NONE',  ( -20.38718376954965450, 37.93371258244203403, -139.5095340218612137 ) ) ;
#361 = VERTEX_POINT ( 'NONE', #4450 ) ;
#362 = AXIS2_PLACEMENT_3D ( 'NONE', #6405, #22711, #20943 ) ;
#363 = EDGE_CURVE ( 'NONE', #23049, #12941, #18964, .T. ) ;
#364 = DIRECTION ( 'NONE',  ( -1.458135199840000066E-12, 1.723066134159999823E-12, 1.000000000000000000 ) ) ;
#365 = VECTOR ( 'NONE', #6982, 1000.000000000000000 ) ;
#366 = DIRECTION ( 'NONE',  ( 1.000000000000000000, 0.000000000000000000, -2.259525899719999991E-12 ) ) ;
#367 = LINE ( 'NONE', #7607, #22136 ) ;
#368 = EDGE_CURVE ( 'NONE', #19467, #13247, #8432, .T. ) ;
#369 = DIRECTION ( 'NONE',  ( -2.839308199620000013E-14, -3.568879590630000244E-13, -1.000000000000000000 ) ) ;
#370 = ORIENTED_EDGE ( 'NONE', *, *, #23215, .F. ) ;
#371 = CARTESIAN_POINT ( 'NONE',  ( 11.65767356897135443, -20.23976850042090092, -148.5552959529999839 ) ) ;
#372 = DIRECTION ( 'NONE',  ( 0.000000000000000000, -1.000000000000000000, 0.000000000000000000 ) ) ;
#373 = ORIENTED_EDGE ( 'NONE', *, *, #23141, .T. ) ;
#374 = EDGE_CURVE ( 'NONE', #19550, #16183, #12819, .T. ) ;
#375 = VECTOR ( 'NONE', #11766, 1000.000000000000000 ) ;
#376 = EDGE_LOOP ( 'NONE', ( #19580, #5131, #12195, #4247 ) ) ;
#377 = EDGE_CURVE ( 'NONE', #16716, #11246, #12757, .T. ) ;
#378 = AXIS2_PLACEMENT_3D ( 'NONE', #21148, #3175, #6615 ) ;
#379 = CARTESIAN_POINT ( 'NONE',  ( 5.809749477036856291, -2.742473698248191649, -136.0552959530131432 ) ) ;
#380 = DIRECTION ( 'NONE',  ( 0.000000000000000000, 1.000000000000000000, 0.000000000000000000 ) ) ;
#381 = VECTOR ( 'NONE', #5006, 1000.000000000000000 ) ;
#382 = DIRECTION ( 'NONE',  ( -1.000000000000000000, -3.994014902950000436E-29, 0.000000000000000000 ) ) ;
#383 = CARTESIAN_POINT ( 'NONE',  ( 7.660612262366659486, 35.75684693635999878, -141.8862908784325612 ) ) ;
#384 = VERTEX_POINT ( 'NONE', #10964 ) ;
#385 = FILL_AREA_STYLE_COLOUR ( '', #1433 ) ;
#386 = CARTESIAN_POINT ( 'NONE',  ( -19.44179523432628898, 36.07285822990824897, -139.5501647635505265 ) ) ;
#387 = EDGE_CURVE ( 'NONE', #598, #15229, #5528, .T. ) ;
#388 = CARTESIAN_POINT ( 'NONE',  ( 10.68320006080000084, -20.50000000000000000, -148.5552959529999839 ) ) ;
#389 = CARTESIAN_POINT ( 'NONE',  ( -9.032885736824702860, 36.94161628544370046, -147.5965110586934941 ) ) ;
#390 = CARTESIAN_POINT ( 'NONE',  ( -24.12417792002877803, 37.90708835554210765, -148.6276364009957547 ) ) ;
#391 = EDGE_CURVE ( 'NONE', #6962, #16283, #23127, .T. ) ;
#392 = LINE ( 'NONE', #16802, #3859 ) ;
#393 = EDGE_CURVE ( 'NONE', #3553, #18415, #4640, .T. ) ;
#394 = ADVANCED_FACE ( 'NONE', ( #1724 ), #9053, .F. ) ;
#395 = CARTESIAN_POINT ( 'NONE',  ( -35.07300000000000040, 14.00000000000000000, -144.5552959529999839 ) ) ;
#396 = DIRECTION ( 'NONE',  ( 2.257157423930000049E-12, 0.000000000000000000, 1.000000000000000000 ) ) ;
#397 = LINE ( 'NONE', #13222, #12316 ) ;
#398 = VECTOR ( 'NONE', #22428, 1000.000000000000000 ) ;
#399 =( BOUNDED_CURVE ( )  B_SPLINE_CURVE ( 5, ( #9681, #664, #13385, #7895, #20653, #2571 ),
 .UNSPECIFIED., .F., .F. ) 
 B_SPLINE_CURVE_WITH_KNOTS ( ( 6, 6 ),
 ( 1.570796326503991924, 3.141592653590000062 ),
 .UNSPECIFIED. ) 
 CURVE ( )  GEOMETRIC_REPRESENTATION_ITEM ( )  RATIONAL_B_SPLINE_CURVE ( ( 0.2500000000000000555, 0.2499999999629477221, 0.2999999999444215582, 0.3999999999258954109, 0.5999999999258953665, 1.000000000000000000 ) ) 
 REPRESENTATION_ITEM ( '' )  );
#400 = CIRCLE ( 'NONE', #3432, 2.999999999999999112 ) ;
#401 = ORIENTED_EDGE ( 'NONE', *, *, #15313, .F. ) ;
#402 = VECTOR ( 'NONE', #1864, 1000.000000000000000 ) ;
#403 = CARTESIAN_POINT ( 'NONE',  ( -5.935706415042687034, 40.05508565971382495, -145.7977461092045530 ) ) ;
#404 = VERTEX_POINT ( 'NONE', #21825 ) ;
#405 = CYLINDRICAL_SURFACE ( 'NONE', #14494, 8.176568160360000448 ) ;
#406 = CARTESIAN_POINT ( 'NONE',  ( -22.02234931426594144, 33.75799147763578389, -142.0591516048408778 ) ) ;
#407 = DIRECTION ( 'NONE',  ( 0.000000000000000000, 1.000000000000000000, 0.000000000000000000 ) ) ;
#408 = EDGE_LOOP ( 'NONE', ( #769, #22028, #13806, #15745 ) ) ;
#409 = CARTESIAN_POINT ( 'NONE',  ( -13.09722452613436516, 33.49976389652860576, -143.7852608042046256 ) ) ;
#410 = CARTESIAN_POINT ( 'NONE',  ( -7.129475577410000042, -25.57825421080000083, -144.0552959529999839 ) ) ;
#411 = LINE ( 'NONE', #11098, #5597 ) ;
#412 = DIRECTION ( 'NONE',  ( 0.000000000000000000, -1.000000000000000000, 0.000000000000000000 ) ) ;
#413 = AXIS2_PLACEMENT_3D ( 'NONE', #5702, #16070, #23326 ) ;
#414 = DIRECTION ( 'NONE',  ( 1.000000000000000000, 0.000000000000000000, 0.000000000000000000 ) ) ;
#415 = DIRECTION ( 'NONE',  ( 2.259525899719999991E-12, 0.000000000000000000, 1.000000000000000000 ) ) ;
#416 = VERTEX_POINT ( 'NONE', #16342 ) ;
#417 = EDGE_CURVE ( 'NONE', #16549, #12948, #12397, .T. ) ;
#418 = PLANE ( 'NONE',  #1885 ) ;
#419 = EDGE_LOOP ( 'NONE', ( #6689, #18751, #11885, #12680 ) ) ;
#420 = SURFACE_STYLE_FILL_AREA ( #21849 ) ;
#421 = ORIENTED_EDGE ( 'NONE', *, *, #10231, .T. ) ;
#422 = CARTESIAN_POINT ( 'NONE',  ( -13.71246964740000074, 35.06639867129999999, -139.8243480419999685 ) ) ;
#423 = CARTESIAN_POINT ( 'NONE',  ( -9.285539185979999388, 35.09287230280000358, -147.9937876190000168 ) ) ;
#424 = CYLINDRICAL_SURFACE ( 'NONE', #5833, 1.500000000000001332 ) ;
#425 = ORIENTED_EDGE ( 'NONE', *, *, #10973, .F. ) ;
#426 = FACE_OUTER_BOUND ( 'NONE', #14985, .T. ) ;
#427 = CARTESIAN_POINT ( 'NONE',  ( 19.45666326950000169, 50.88169314249999786, -136.0552959530000123 ) ) ;
#428 = AXIS2_PLACEMENT_3D ( 'NONE', #17687, #19484, #10762 ) ;
#429 = FACE_OUTER_BOUND ( 'NONE', #6250, .T. ) ;
#430 = VECTOR ( 'NONE', #16605, 1000.000000000000000 ) ;
#431 = ORIENTED_EDGE ( 'NONE', *, *, #17551, .T. ) ;
#432 = CARTESIAN_POINT ( 'NONE',  ( -20.83898962464882842, 39.06148406400365758, -147.0165715935449953 ) ) ;
#433 = CARTESIAN_POINT ( 'NONE',  ( 9.756656435460874022, 37.81905845387217369, -141.6932697408578576 ) ) ;
#434 = DIRECTION ( 'NONE',  ( -1.000000000000000000, 0.000000000000000000, 0.000000000000000000 ) ) ;
#435 = DIRECTION ( 'NONE',  ( 0.000000000000000000, 1.603797727410000024E-26, -1.000000000000000000 ) ) ;
#436 = ORIENTED_EDGE ( 'NONE', *, *, #7654, .T. ) ;
#437 = EDGE_CURVE ( 'NONE', #3022, #18237, #5403, .T. ) ;
#438 = CYLINDRICAL_SURFACE ( 'NONE', #17527, 2.999999999999999112 ) ;
#439 = ORIENTED_EDGE ( 'NONE', *, *, #4229, .F. ) ;
#440 = ADVANCED_FACE ( 'NONE', ( #21467 ), #14562, .T. ) ;
#441 = VECTOR ( 'NONE', #15364, 1000.000000000000000 ) ;
#442 = CLOSED_SHELL ( 'NONE', ( #9324, #14762, #13056, #18672, #19728, #11827, #3231, #1555, #8168, #17761, #5900, #20748, #17875, #12551, #6898, #10761, #21469, #15064, #5744, #9048, #10757, #19124, #8783, #16660, #5435, #11889, #2238, #21621, #10384, #1685, #10160, #18102, #2306, #16052, #22700, #15391, #3799, #8755, #18283, #22183, #12588, #7262, #14355, #653, #22347, #13377, #4882, #10197, #21282, #7768, #18410, #22521, #11400, #16358, #23317, #3120, #7355, #13403, #22544, #7833, #8957, #20415, #19258, #523, #5604, #17631, #20506, #5512, #10979, #8075, #2679, #9354, #4586, #22200, #23359, #17607, #5542, #23499, #15096, #7365, #9624, #7391, #20151, #23430, #18033, #13348, #7151, #11366, #4409, #5104, #2402, #2042, #18132, #10666, #7930, #20884, #13762, #18713, #18695, #14321, #2065, #14378, #15647, #17406, #4519, #4684, #3694, #21015, #20879, #11134, #7412, #2812, #10561, #7625, #18912, #19316, #9573, #6767, #17249, #18227, #4140, #23025, #5289, #14520, #11229, #648, #6454, #12373, #19083, #6624, #17899, #15037, #11061, #12004, #20941, #16351, #7440, #9553, #16817, #17324, #7025, #19114, #16510, #11613, #13749, #6389, #5831, #9940, #12623, #14887, #20445, #13941, #17758, #16749, #22349, #22437, #10217, #1808, #15771, #12918, #17075, #2483, #7067, #6285, #19351 ) ) ;
#443 = AXIS2_PLACEMENT_3D ( 'NONE', #17861, #20351, #4284 ) ;
#444 = ORIENTED_EDGE ( 'NONE', *, *, #1007, .T. ) ;
#445 = CARTESIAN_POINT ( 'NONE',  ( -26.83129905141586846, 39.07913712597448352, -146.9590705472632521 ) ) ;
#446 = ORIENTED_EDGE ( 'NONE', *, *, #8608, .F. ) ;
#447 = CARTESIAN_POINT ( 'NONE',  ( -23.44935120326739764, 36.05472785596497687, -139.7839751993253685 ) ) ;
#448 = B_SPLINE_CURVE_WITH_KNOTS ( 'NONE', 5,
 ( #16535, #590, #18437, #5588, #12836, #20113, #242, #2960, #2732, #6397, #21052, #13899 ),
 .UNSPECIFIED., .F., .F.,
 ( 6, 3, 3, 6 ),
 ( 0.000000000000000000, 4.124045064660000648, 8.344666563069999654, 12.67057240369999782 ),
 .UNSPECIFIED. ) ;
#449 = ORIENTED_EDGE ( 'NONE', *, *, #3663, .T. ) ;
#450 = CARTESIAN_POINT ( 'NONE',  ( -16.51085694111268865, -45.62135916506277056, -150.0552959529999555 ) ) ;
#451 = ORIENTED_EDGE ( 'NONE', *, *, #12079, .F. ) ;
#452 = APPLICATION_PROTOCOL_DEFINITION ( 'draft international standard', 'automotive_design', 1998, #14356 ) ;
#453 = ORIENTED_EDGE ( 'NONE', *, *, #12083, .T. ) ;
#454 = CARTESIAN_POINT ( 'NONE',  ( -27.67795712710000089, 37.78351609900000341, -147.6208067679999942 ) ) ;
#455 = DIRECTION ( 'NONE',  ( -1.000000000000000000, 0.000000000000000000, 0.000000000000000000 ) ) ;
#456 = LINE ( 'NONE', #20555, #2007 ) ;
#457 = CARTESIAN_POINT ( 'NONE',  ( 19.91945158500000090, -51.14507942810000429, -149.5552959529999839 ) ) ;
#458 = CYLINDRICAL_SURFACE ( 'NONE', #11391, 10.00000000000000888 ) ;
#459 = CARTESIAN_POINT ( 'NONE',  ( -8.767025672889793952, 38.73734267217074034, -139.9349420084332962 ) ) ;
#460 = EDGE_LOOP ( 'NONE', ( #22587, #8189, #13653, #11072, #16704 ) ) ;
#461 = LINE ( 'NONE', #9594, #4132 ) ;
#462 = AXIS2_PLACEMENT_3D ( 'NONE', #6637, #9837, #21169 ) ;
#463 = VECTOR ( 'NONE', #13106, 999.9999999999998863 ) ;
#464 = AXIS2_PLACEMENT_3D ( 'NONE', #871, #514, #22275 ) ;
#465 = CARTESIAN_POINT ( 'NONE',  ( -22.10824191589999899, -32.00000000000000000, -146.2257682199999920 ) ) ;
#466 = CARTESIAN_POINT ( 'NONE',  ( -25.90907760989737341, 37.01347911741230945, -139.4251635482864913 ) ) ;
#467 = VERTEX_POINT ( 'NONE', #15986 ) ;
#468 = DIRECTION ( 'NONE',  ( -1.000000000000000000, 0.000000000000000000, 0.000000000000000000 ) ) ;
#469 = CARTESIAN_POINT ( 'NONE',  ( -11.91401949022731799, 39.67431894273512683, -140.4170659721649486 ) ) ;
#470 = EDGE_CURVE ( 'NONE', #2284, #2388, #4261, .T. ) ;
#471 = CARTESIAN_POINT ( 'NONE',  ( -17.79289316922850617, 37.75490432960187803, -147.9677353736447571 ) ) ;
#472 = CARTESIAN_POINT ( 'NONE',  ( 22.68320006080000084, -34.50000000000000000, -148.5552959529999839 ) ) ;
#473 = VERTEX_POINT ( 'NONE', #1610 ) ;
#474 = CARTESIAN_POINT ( 'NONE',  ( -7.572469997240619755, 37.05365869150052305, -139.6601318952005215 ) ) ;
#475 = ADVANCED_FACE ( 'NONE', ( #8830 ), #16110, .F. ) ;
#476 = CARTESIAN_POINT ( 'NONE',  ( -30.64259443220337786, 40.28463426600031028, -145.8661425198801567 ) ) ;
#477 = VERTEX_POINT ( 'NONE', #7171 ) ;
#478 = FACE_OUTER_BOUND ( 'NONE', #722, .T. ) ;
#479 = CARTESIAN_POINT ( 'NONE',  ( 22.50000000000000000, 33.50000000000000000, -150.0552959529999839 ) ) ;
#480 = ORIENTED_EDGE ( 'NONE', *, *, #12943, .T. ) ;
#481 = PLANE ( 'NONE',  #12091 ) ;
#482 = CARTESIAN_POINT ( 'NONE',  ( -20.97542662470000252, 40.85881720449999932, -141.8340754020000247 ) ) ;
#483 = COLOUR_RGB ( '', 0.09019608, 0.27058824, 0.51372549) ;
#484 = ORIENTED_EDGE ( 'NONE', *, *, #15490, .T. ) ;
#485 = PRESENTATION_STYLE_ASSIGNMENT (( #16769 ) ) ;
#486 = AXIS2_PLACEMENT_3D ( 'NONE', #13907, #11751, #12111 ) ;
#487 = DIRECTION ( 'NONE',  ( -0.9848077530125620704, 4.409131086918041429E-28, -0.1736481776649230480 ) ) ;
#488 = DIRECTION ( 'NONE',  ( 0.000000000000000000, 2.256894259950000208E-12, -1.000000000000000000 ) ) ;
#489 = ORIENTED_EDGE ( 'NONE', *, *, #10165, .F. ) ;
#490 = LINE ( 'NONE', #2397, #14405 ) ;
#491 = DIRECTION ( 'NONE',  ( 1.000000000000000000, 0.000000000000000000, 2.516505522483685870E-12 ) ) ;
#492 = CARTESIAN_POINT ( 'NONE',  ( -5.499999999960005326, 44.23441892295438294, -136.0552959529876205 ) ) ;
#493 = ORIENTED_EDGE ( 'NONE', *, *, #2717, .F. ) ;
#494 = DIRECTION ( 'NONE',  ( 8.955190032050000935E-12, -9.104778821549999739E-13, 1.000000000000000000 ) ) ;
#495 = CARTESIAN_POINT ( 'NONE',  ( -15.39067985669018235, -44.46175622020449225, -136.0552959529652526 ) ) ;
#496 = ORIENTED_EDGE ( 'NONE', *, *, #9897, .T. ) ;
#497 = EDGE_CURVE ( 'NONE', #7372, #10073, #14436, .T. ) ;
#498 = MECHANICAL_DESIGN_GEOMETRIC_PRESENTATION_REPRESENTATION (  '', ( #20638 ), #15318 ) ;
#499 = ORIENTED_EDGE ( 'NONE', *, *, #14733, .F. ) ;
#500 = AXIS2_PLACEMENT_3D ( 'NONE', #8679, #15962, #22989 ) ;
#501 = LINE ( 'NONE', #11416, #1400 ) ;
#502 = CARTESIAN_POINT ( 'NONE',  ( -7.500000000000000000, 48.50000000000000000, -150.5552959529999839 ) ) ;
#503 = CARTESIAN_POINT ( 'NONE',  ( 31.50000000000000000, -21.03620104879999886, -136.0552959530000123 ) ) ;
#504 = CARTESIAN_POINT ( 'NONE',  ( 7.911979894106841549, 35.62004518156074795, -141.9706744367260853 ) ) ;
#505 = ORIENTED_EDGE ( 'NONE', *, *, #9782, .F. ) ;
#506 = EDGE_CURVE ( 'NONE', #3901, #16131, #13345, .T. ) ;
#507 = DIRECTION ( 'NONE',  ( -0.7633862853691872896, 0.6459422414660880296, 5.370703881624201706E-14 ) ) ;
#508 = LINE ( 'NONE', #2417, #23112 ) ;
#509 = CARTESIAN_POINT ( 'NONE',  ( -9.072898850179999641, 36.94639249900000522, -148.2684494029999769 ) ) ;
#510 = CARTESIAN_POINT ( 'NONE',  ( -22.88190335430070377, 39.79040966463082185, -140.3815034252083365 ) ) ;
#511 = CARTESIAN_POINT ( 'NONE',  ( -15.46613156833100078, 36.99333119719623397, -147.5584717933785726 ) ) ;
#512 = ADVANCED_FACE ( 'NONE', ( #5969 ), #11083, .F. ) ;
#513 = EDGE_CURVE ( 'NONE', #11545, #10772, #7749, .T. ) ;
#514 = DIRECTION ( 'NONE',  ( 0.000000000000000000, 0.000000000000000000, -1.000000000000000000 ) ) ;
#515 = CARTESIAN_POINT ( 'NONE',  ( -12.50000000000000000, 42.50000000000000000, -150.5552959529999839 ) ) ;
#516 = PRODUCT_DEFINITION_FORMATION_WITH_SPECIFIED_SOURCE ( 'ANY', '', #19655, .NOT_KNOWN. ) ;
#517 = DIRECTION ( 'NONE',  ( 0.000000000000000000, 0.000000000000000000, 1.000000000000000000 ) ) ;
#518 = ORIENTED_EDGE ( 'NONE', *, *, #18360, .T. ) ;
#519 = CARTESIAN_POINT ( 'NONE',  ( -7.081915218180248495, 37.06683495600064759, -147.7519347211647585 ) ) ;
#520 = DIRECTION ( 'NONE',  ( -1.000000000000000000, 0.000000000000000000, 0.000000000000000000 ) ) ;
#521 = EDGE_LOOP ( 'NONE', ( #17341, #16044, #20212, #9730 ) ) ;
#522 = DIRECTION ( 'NONE',  ( 0.000000000000000000, 1.000000000000000000, -2.273736754430000208E-12 ) ) ;
#523 = ADVANCED_FACE ( 'NONE', ( #5738 ), #15015, .T. ) ;
#524 = EDGE_CURVE ( 'NONE', #12078, #6964, #6093, .T. ) ;
#525 = CARTESIAN_POINT ( 'NONE',  ( -22.51542269368358617, 35.01159793962629863, -141.2271873608204373 ) ) ;
#526 = LINE ( 'NONE', #3858, #17814 ) ;
#527 = ORIENTED_EDGE ( 'NONE', *, *, #524, .F. ) ;
#528 = CARTESIAN_POINT ( 'NONE',  ( -12.51319725274692374, 36.30635479524141829, -147.4212986608875156 ) ) ;
#529 = EDGE_CURVE ( 'NONE', #13555, #22754, #79, .T. ) ;
#530 = CARTESIAN_POINT ( 'NONE',  ( -6.547730170579999509, -18.66441632429999942, -147.5552959529999839 ) ) ;
#531 = EDGE_CURVE ( 'NONE', #22008, #18104, #14787, .T. ) ;
#532 = LINE ( 'NONE', #16579, #17364 ) ;
#533 = FACE_OUTER_BOUND ( 'NONE', #22449, .T. ) ;
#534 = LINE ( 'NONE', #4213, #23018 ) ;
#535 = CARTESIAN_POINT ( 'NONE',  ( -13.59981317924083655, 37.05039483956776536, -139.6306434366684925 ) ) ;
#536 =( REPRESENTATION_RELATIONSHIP ('NONE','NONE', #7672, #15879 ) REPRESENTATION_RELATIONSHIP_WITH_TRANSFORMATION ( #16821 )SHAPE_REPRESENTATION_RELATIONSHIP( ) );
#537 = VERTEX_POINT ( 'NONE', #18717 ) ;
#538 = SHAPE_REPRESENTATION ( 'Latch Bolt Assembly', ( #5025 ), #7334 ) ;
#539 = CARTESIAN_POINT ( 'NONE',  ( -27.92684401174140163, 34.15387849089756145, -147.9120013265362559 ) ) ;
#540 = ORIENTED_EDGE ( 'NONE', *, *, #741, .F. ) ;
#541 = PRESENTATION_STYLE_ASSIGNMENT (( #8237 ) ) ;
#542 = ORIENTED_EDGE ( 'NONE', *, *, #17707, .F. ) ;
#543 = CARTESIAN_POINT ( 'NONE',  ( -13.13790626639999992, 32.38985286280000508, -143.7114742199999853 ) ) ;
#544 = DIRECTION ( 'NONE',  ( 1.000000000000000000, 0.000000000000000000, 0.000000000000000000 ) ) ;
#545 = DIRECTION ( 'NONE',  ( 0.000000000000000000, -0.8660254037841379482, 0.5000000000005210277 ) ) ;
#546 = VERTEX_POINT ( 'NONE', #2424 ) ;
#547 = DIRECTION ( 'NONE',  ( -2.257144641399999941E-12, 0.000000000000000000, -1.000000000000000000 ) ) ;
#548 = DIRECTION ( 'NONE',  ( 0.000000000000000000, 0.000000000000000000, 1.000000000000000000 ) ) ;
#549 = ORIENTED_EDGE ( 'NONE', *, *, #9148, .T. ) ;
#550 = CARTESIAN_POINT ( 'NONE',  ( -19.79317654000728055, 38.64314174751988418, -140.5356700201026001 ) ) ;
#551 = EDGE_CURVE ( 'NONE', #19314, #16041, #18247, .T. ) ;
#552 = VECTOR ( 'NONE', #14058, 1000.000000000000000 ) ;
#553 = CARTESIAN_POINT ( 'NONE',  ( 9.088020105981311048, 38.37995481845652535, -141.9706744367346118 ) ) ;
#554 = EDGE_CURVE ( 'NONE', #10724, #2155, #2183, .T. ) ;
#555 = DIRECTION ( 'NONE',  ( -1.000000000000000000, 0.000000000000000000, 1.701177084980000217E-20 ) ) ;
#556 = DIRECTION ( 'NONE',  ( 0.000000000000000000, -1.000000000000000000, 0.000000000000000000 ) ) ;
#557 = ORIENTED_EDGE ( 'NONE', *, *, #5693, .F. ) ;
#558 = DIRECTION ( 'NONE',  ( 0.05349466063429310358, 0.9985681355238719137, -1.093104632299860501E-13 ) ) ;
#559 = ORIENTED_EDGE ( 'NONE', *, *, #6683, .T. ) ;
#560 = DIRECTION ( 'NONE',  ( 0.000000000000000000, -1.000000000000000000, 0.000000000000000000 ) ) ;
#561 = ORIENTED_EDGE ( 'NONE', *, *, #19, .F. ) ;
#562 = CARTESIAN_POINT ( 'NONE',  ( -25.64792992871999999, 37.04465132566515706, -139.7265440085297996 ) ) ;
#563 = EDGE_LOOP ( 'NONE', ( #12365, #15477, #17819, #6056 ) ) ;
#564 = LINE ( 'NONE', #18409, #4525 ) ;
#565 = VERTEX_POINT ( 'NONE', #11308 ) ;
#566 = CARTESIAN_POINT ( 'NONE',  ( -15.39269908169871393, -46.00000000000000000, -150.0552959529999839 ) ) ;
#567 = VERTEX_POINT ( 'NONE', #9642 ) ;
#568 = ORIENTED_EDGE ( 'NONE', *, *, #21534, .F. ) ;
#569 = CARTESIAN_POINT ( 'NONE',  ( 4.352290413739999586, -26.01556969399999986, -145.5552959529999839 ) ) ;
#570 = CARTESIAN_POINT ( 'NONE',  ( 19.13369214859999801, 51.50000000000000000, -142.8052959529999839 ) ) ;
#571 = DIRECTION ( 'NONE',  ( 1.000000000000000000, 0.000000000000000000, -2.255897967639999903E-12 ) ) ;
#572 = CYLINDRICAL_SURFACE ( 'NONE', #7900, 2.500000000000001776 ) ;
#573 = CARTESIAN_POINT ( 'NONE',  ( -6.366122344970272628, 35.09376510157478180, -148.3726825278031640 ) ) ;
#574 = EDGE_CURVE ( 'NONE', #10851, #1178, #9171, .T. ) ;
#575 = FACE_OUTER_BOUND ( 'NONE', #12604, .T. ) ;
#576 = VERTEX_POINT ( 'NONE', #16915 ) ;
#577 = DIRECTION ( 'NONE',  ( 0.000000000000000000, -1.000000000000000000, 0.000000000000000000 ) ) ;
#578 = CARTESIAN_POINT ( 'NONE',  ( -6.264930628975839966, -16.71491984542973341, -147.5552959529461816 ) ) ;
#579 = VECTOR ( 'NONE', #12352, 1000.000000000000114 ) ;
#580 = DIRECTION ( 'NONE',  ( 1.000000000000000000, 0.000000000000000000, -1.522591576628786004E-13 ) ) ;
#581 = ORIENTED_EDGE ( 'NONE', *, *, #16197, .T. ) ;
#582 = CARTESIAN_POINT ( 'NONE',  ( -12.41748666345656282, 41.11124952250558096, -146.5209369397300918 ) ) ;
#583 = CARTESIAN_POINT ( 'NONE',  ( -18.01836706189362758, 38.92693601672081627, -148.4107366658697913 ) ) ;
#584 = CARTESIAN_POINT ( 'NONE',  ( -29.86462848822639771, 41.46897301220559484, -145.0541174283626162 ) ) ;
#585 = EDGE_LOOP ( 'NONE', ( #1690, #3105, #11478, #4390 ) ) ;
#586 = CARTESIAN_POINT ( 'NONE',  ( -6.518232409689999507, 33.41592120480000006, -146.1606736330000160 ) ) ;
#587 = DIRECTION ( 'NONE',  ( 1.000000000000000000, 0.000000000000000000, -2.257120985840000117E-12 ) ) ;
#588 = ORIENTED_EDGE ( 'NONE', *, *, #13323, .F. ) ;
#589 = LINE ( 'NONE', #22831, #9470 ) ;
#590 = CARTESIAN_POINT ( 'NONE',  ( -17.32451618079999633, 37.89224186959999940, -139.5945780149999962 ) ) ;
#591 = EDGE_LOOP ( 'NONE', ( #2730, #14318, #830, #3927 ) ) ;
#592 = B_SPLINE_CURVE_WITH_KNOTS ( 'NONE', 3,
 ( #5537, #12672, #3987, #14821, #23392, #9212, #11220, #12786, #18494, #18153, #10755, #16137, #18038, #20057, #8972, #21737, #5427, #19939 ),
 .UNSPECIFIED., .F., .F.,
 ( 4, 2, 2, 2, 2, 2, 2, 2, 4 ),
 ( 0.000000000000000000, 0.1249999999999998057, 0.2499999999999998335, 0.3749999999999998335, 0.4999999999999998890, 0.6249999999999998890, 0.7499999999999998890, 0.8750000000000000000, 1.000000000000000000 ),
 .UNSPECIFIED. ) ;
#593 = LINE ( 'NONE', #4279, #23134 ) ;
#594 = CARTESIAN_POINT ( 'NONE',  ( -19.90747643769189423, 40.84829927215759682, -141.9758135236385783 ) ) ;
#595 = ORIENTED_EDGE ( 'NONE', *, *, #22542, .F. ) ;
#596 = CARTESIAN_POINT ( 'NONE',  ( -27.80359210614968291, 32.89696731216636039, -146.3345487532903917 ) ) ;
#597 = DIRECTION ( 'NONE',  ( 1.000000000000000000, -2.312964634635743450E-15, -2.257453483404485639E-12 ) ) ;
#598 = VERTEX_POINT ( 'NONE', #7861 ) ;
#599 = DIRECTION ( 'NONE',  ( 4.430318231640945063E-12, -6.100259101492280662E-13, 1.000000000000000000 ) ) ;
#600 = VECTOR ( 'NONE', #18376, 1000.000000000000000 ) ;
#601 = DIRECTION ( 'NONE',  ( 0.000000000000000000, 0.000000000000000000, 1.000000000000000000 ) ) ;
#602 = CIRCLE ( 'NONE', #14284, 0.5000000000000004441 ) ;
#603 = CARTESIAN_POINT ( 'NONE',  ( -22.10824191589623666, -4.196349540848737014, -146.3157682190018818 ) ) ;
#604 = EDGE_LOOP ( 'NONE', ( #581, #786, #19949, #21046 ) ) ;
#605 = EDGE_CURVE ( 'NONE', #4355, #13765, #9291, .T. ) ;
#606 = CARTESIAN_POINT ( 'NONE',  ( -19.79184979336555017, 37.02747215728111740, -140.6521846888478819 ) ) ;
#607 = CARTESIAN_POINT ( 'NONE',  ( -30.49999999990000177, 29.00000000000000000, -147.5552959529999839 ) ) ;
#608 = EDGE_CURVE ( 'NONE', #14496, #2454, #1959, .T. ) ;
#609 = ORIENTED_EDGE ( 'NONE', *, *, #18363, .F. ) ;
#610 = EDGE_LOOP ( 'NONE', ( #15097, #4156, #2830, #8303 ) ) ;
#611 = CARTESIAN_POINT ( 'NONE',  ( 5.701130924195719096, -2.579771545651550646, -136.0552959530129158 ) ) ;
#612 = LINE ( 'NONE', #730, #5551 ) ;
#613 = CARTESIAN_POINT ( 'NONE',  ( 32.00000000000000000, 32.96379895120000469, -136.0552959530000123 ) ) ;
#614 = CARTESIAN_POINT ( 'NONE',  ( 7.393053867465662954, 35.98765375272272848, -141.7694449707084914 ) ) ;
#615 = VECTOR ( 'NONE', #5815, 1000.000000000000000 ) ;
#616 = ORIENTED_EDGE ( 'NONE', *, *, #4162, .T. ) ;
#617 = CARTESIAN_POINT ( 'NONE',  ( 32.50000000000000000, -21.03620104879999886, -136.5552959530000123 ) ) ;
#618 = AXIS2_PLACEMENT_3D ( 'NONE', #10592, #19305, #3240 ) ;
#619 = DIRECTION ( 'NONE',  ( -1.525446435830000185E-13, -8.171241461240000022E-13, -1.000000000000000000 ) ) ;
#620 = EDGE_CURVE ( 'NONE', #20642, #4666, #18468, .T. ) ;
#621 = DIRECTION ( 'NONE',  ( 1.000000000000000000, 0.000000000000000000, -4.510774274160000731E-12 ) ) ;
#622 = FACE_OUTER_BOUND ( 'NONE', #19220, .T. ) ;
#623 = PLANE ( 'NONE',  #6012 ) ;
#624 = LINE ( 'NONE', #7513, #10296 ) ;
#625 = CARTESIAN_POINT ( 'NONE',  ( -16.48779918059999616, 32.42295671489999620, -143.3618442240000093 ) ) ;
#626 = CARTESIAN_POINT ( 'NONE',  ( -32.50000000000000000, 27.00000000000000000, -141.5552959529999839 ) ) ;
#627 = DIRECTION ( 'NONE',  ( 0.9990052710704846461, -0.04459224566432164194, -1.160036675700561719E-13 ) ) ;
#628 = CARTESIAN_POINT ( 'NONE',  ( 12.50000000010000001, 24.10555127549999810, -150.5552959529999839 ) ) ;
#629 = ORIENTED_EDGE ( 'NONE', *, *, #11116, .F. ) ;
#630 = CARTESIAN_POINT ( 'NONE',  ( -5.700500667576763547, 40.41662643729544868, -143.6588243170081682 ) ) ;
#631 = CARTESIAN_POINT ( 'NONE',  ( -6.366307851350000213, -50.50000000000000000, -136.0552959530000123 ) ) ;
#632 = VECTOR ( 'NONE', #2081, 1000.000000000000114 ) ;
#633 = EDGE_CURVE ( 'NONE', #11242, #11916, #16457, .T. ) ;
#634 = VERTEX_POINT ( 'NONE', #9534 ) ;
#635 = CARTESIAN_POINT ( 'NONE',  ( -21.59125871610556402, 33.71934651132892924, -145.8354015992185850 ) ) ;
#636 = FACE_OUTER_BOUND ( 'NONE', #14587, .T. ) ;
#637 = ORIENTED_EDGE ( 'NONE', *, *, #7410, .T. ) ;
#638 = CARTESIAN_POINT ( 'NONE',  ( -12.69103652210661615, 35.00128951864121518, -146.9022827771903223 ) ) ;
#639 = PLANE ( 'NONE',  #16943 ) ;
#640 = ADVANCED_FACE ( 'NONE', ( #7633, #14906 ), #22163, .F. ) ;
#641 = CARTESIAN_POINT ( 'NONE',  ( 6.500000000000000000, 13.00000000000000000, -150.0552959529999839 ) ) ;
#642 = DIRECTION ( 'NONE',  ( 0.9990052710704846461, -0.04459224566432164194, -1.160036675700561719E-13 ) ) ;
#643 = CARTESIAN_POINT ( 'NONE',  ( -2.499999999940000439, 42.50000000000000000, -144.0552959529999839 ) ) ;
#644 = DIRECTION ( 'NONE',  ( 0.000000000000000000, -1.000000000000000000, 0.000000000000000000 ) ) ;
#645 = ORIENTED_EDGE ( 'NONE', *, *, #21775, .T. ) ;
#646 = VECTOR ( 'NONE', #14333, 1000.000000000000000 ) ;
#647 =( NAMED_UNIT ( * ) SI_UNIT ( $, .STERADIAN. ) SOLID_ANGLE_UNIT ( ) );
#648 = ADVANCED_FACE ( 'NONE', ( #7405 ), #14667, .F. ) ;
#649 = ORIENTED_EDGE ( 'NONE', *, *, #19647, .F. ) ;
#650 = CARTESIAN_POINT ( 'NONE',  ( -12.79720822650000045, 32.99715178900000012, -146.4964997610000239 ) ) ;
#651 = CARTESIAN_POINT ( 'NONE',  ( -10.56415788819999868, 36.18163687389999694, -139.7056672729999889 ) ) ;
#652 = CARTESIAN_POINT ( 'NONE',  ( -4.499999999939999995, 34.80604359529999670, -142.8567321060000097 ) ) ;
#653 = ADVANCED_FACE ( 'NONE', ( #8333 ), #17029, .T. ) ;
#654 = ORIENTED_EDGE ( 'NONE', *, *, #11108, .F. ) ;
#655 = DIRECTION ( 'NONE',  ( 2.839308199620000013E-14, 3.568879590630000244E-13, 1.000000000000000000 ) ) ;
#656 = FACE_OUTER_BOUND ( 'NONE', #610, .T. ) ;
#657 = ORIENTED_EDGE ( 'NONE', *, *, #277, .T. ) ;
#658 = CARTESIAN_POINT ( 'NONE',  ( -20.74716465872499427, 38.46557005212173408, -140.6515328043094826 ) ) ;
#659 = VECTOR ( 'NONE', #1651, 1000.000000000000000 ) ;
#660 = CARTESIAN_POINT ( 'NONE',  ( 8.914847504438609960, 38.44170426491582049, -142.0128484171024752 ) ) ;
#661 = AXIS2_PLACEMENT_3D ( 'NONE', #17645, #15626, #22893 ) ;
#662 = FACE_BOUND ( 'NONE', #2795, .T. ) ;
#663 = AXIS2_PLACEMENT_3D ( 'NONE', #6976, #3646, #1872 ) ;
#664 = CARTESIAN_POINT ( 'NONE',  ( -22.48976697757458254, 37.06353063726728436, -140.4055699430356015 ) ) ;
#665 = ADVANCED_FACE ( 'NONE', ( #6439 ), #20974, .T. ) ;
#666 = CARTESIAN_POINT ( 'NONE',  ( 32.50000000000000000, -40.50000000000000000, -137.0552959530000123 ) ) ;
#667 = ORIENTED_EDGE ( 'NONE', *, *, #18339, .F. ) ;
#668 = EDGE_CURVE ( 'NONE', #11661, #7563, #4778, .T. ) ;
#669 =( BOUNDED_CURVE ( )  B_SPLINE_CURVE ( 5, ( #13319, #6186, #2623, #22370, #18688, #13085, #2509, #252, #11633, #18446, #20701, #12969 ),
 .UNSPECIFIED., .F., .F. ) 
 B_SPLINE_CURVE_WITH_KNOTS ( ( 6, 3, 3, 6 ),
 ( 0.000000000000000000, 4.570086947620000117, 8.869210483019999813, 12.91901055009999943 ),
 .UNSPECIFIED. ) 
 CURVE ( )  GEOMETRIC_REPRESENTATION_ITEM ( )  RATIONAL_B_SPLINE_CURVE ( ( 0.2500000000000000000, 0.2500000000000000000, 0.2500000000000000000, 0.2500000000000000000, 0.2500000000000000000, 0.2500000000000000000, 0.2500000000000000000, 0.2500000000000000000, 0.2500000000000000000, 0.2500000000000000000, 0.2500000000000000000, 0.2500000000000000000 ) ) 
 REPRESENTATION_ITEM ( '' )  );
#670 = DIRECTION ( 'NONE',  ( 0.000000000000000000, 1.000000000000000000, 0.000000000000000000 ) ) ;
#671 = ORIENTED_EDGE ( 'NONE', *, *, #7862, .F. ) ;
#672 = LINE ( 'NONE', #8257, #20839 ) ;
#674 = EDGE_LOOP ( 'NONE', ( #13508, #15033, #13775, #6801 ) ) ;
#673 = VECTOR ( 'NONE', #22152, 1000.000000000000000 ) ;
#675 = CARTESIAN_POINT ( 'NONE',  ( -27.01837854179119702, 37.68189902554408377, -147.5283965130139734 ) ) ;
#676 = EDGE_CURVE ( 'NONE', #3124, #23083, #5766, .T. ) ;
#677 = ORIENTED_EDGE ( 'NONE', *, *, #6323, .T. ) ;
#678 = CARTESIAN_POINT ( 'NONE',  ( -22.55322464622646805, 32.24327928621291051, -143.4921094554972854 ) ) ;
#679 = EDGE_CURVE ( 'NONE', #5644, #19743, #22116, .T. ) ;
#680 = VECTOR ( 'NONE', #351, 1000.000000000000000 ) ;
#681 = EDGE_LOOP ( 'NONE', ( #5696, #5785, #21336, #12694 ) ) ;
#682 = CARTESIAN_POINT ( 'NONE',  ( -32.50000000000000000, 0.000000000000000000, -150.0552959529999839 ) ) ;
#683 = VERTEX_POINT ( 'NONE', #9754 ) ;
#684 = EDGE_CURVE ( 'NONE', #11278, #7890, #748, .T. ) ;
#685 = ORIENTED_EDGE ( 'NONE', *, *, #13914, .T. ) ;
#686 = CARTESIAN_POINT ( 'NONE',  ( -27.30725598840000146, 40.30964169850000189, -145.9048855949999961 ) ) ;
#687 = DIRECTION ( 'NONE',  ( 0.000000000000000000, -2.256894259950000208E-12, 1.000000000000000000 ) ) ;
#688 = FACE_OUTER_BOUND ( 'NONE', #3217, .T. ) ;
#689 = LINE ( 'NONE', #22455, #8666 ) ;
#690 = CARTESIAN_POINT ( 'NONE',  ( -6.875342432574099050, 34.21798895325673584, -148.0105455186688914 ) ) ;
#691 = CARTESIAN_POINT ( 'NONE',  ( -26.35824191589999899, -1.500000000000000000, -150.0657682190000060 ) ) ;
#692 = EDGE_LOOP ( 'NONE', ( #18060, #16442, #20942, #9453 ) ) ;
#693 = CARTESIAN_POINT ( 'NONE',  ( -1.500000000000000222, 44.76558107705237433, -150.0552959530000123 ) ) ;
#694 = AXIS2_PLACEMENT_3D ( 'NONE', #20611, #4769, #621 ) ;
#695 = CARTESIAN_POINT ( 'NONE',  ( 9.797496117245477976, 37.75936717763469375, -146.4386832613834599 ) ) ;
#696 = PRESENTATION_LAYER_ASSIGNMENT (  '', '', ( #4114 ) ) ;
#697 = CARTESIAN_POINT ( 'NONE',  ( 3.000000000010000001, -3.500000000000000000, -136.0552959530000123 ) ) ;
#698 = ORIENTED_EDGE ( 'NONE', *, *, #6854, .T. ) ;
#699 = CARTESIAN_POINT ( 'NONE',  ( -12.76385253868072134, 37.02886902027827887, -147.6186336933980101 ) ) ;
#700 = CARTESIAN_POINT ( 'NONE',  ( -17.81786398825392581, 37.84862138750237648, -148.3932271983275086 ) ) ;
#701 = CARTESIAN_POINT ( 'NONE',  ( -9.282104535849999394, -16.71402168319999859, -144.5552959529999839 ) ) ;
#702 = EDGE_LOOP ( 'NONE', ( #22951, #2945, #10510, #19739 ) ) ;
#703 = DIRECTION ( 'NONE',  ( 0.1000233216789610108, 0.9949850929136109245, -3.588240815588595806E-13 ) ) ;
#704 = LINE ( 'NONE', #18543, #23404 ) ;
#705 = ORIENTED_EDGE ( 'NONE', *, *, #23377, .F. ) ;
#706 = DIRECTION ( 'NONE',  ( 1.000000000000000000, 0.000000000000000000, -2.257453483404485639E-12 ) ) ;
#707 = DIRECTION ( 'NONE',  ( 0.000000000000000000, -2.257144641399999941E-12, -1.000000000000000000 ) ) ;
#708 = ORIENTED_EDGE ( 'NONE', *, *, #12053, .T. ) ;
#709 = DIRECTION ( 'NONE',  ( 0.000000000000000000, -1.000000000000000000, 2.257144641399999941E-12 ) ) ;
#710 = EDGE_CURVE ( 'NONE', #6873, #1863, #12236, .T. ) ;
#711 = CARTESIAN_POINT ( 'NONE',  ( -21.83774898087361649, 37.96346924979418702, -148.4776379419676857 ) ) ;
#712 = VERTEX_POINT ( 'NONE', #6671 ) ;
#713 = SURFACE_SIDE_STYLE ('',( #19911 ) ) ;
#714 = VECTOR ( 'NONE', #22848, 1000.000000000000000 ) ;
#715 = DIRECTION ( 'NONE',  ( 0.000000000000000000, 1.000000000000000000, 0.000000000000000000 ) ) ;
#716 = VECTOR ( 'NONE', #6030, 1000.000000000000227 ) ;
#717 = ORIENTED_EDGE ( 'NONE', *, *, #2283, .F. ) ;
#718 = LINE ( 'NONE', #13669, #23526 ) ;
#719 = AXIS2_PLACEMENT_3D ( 'NONE', #21200, #4887, #3113 ) ;
#720 = CARTESIAN_POINT ( 'NONE',  ( 24.89581725840000104, -26.85672394480000236, -144.5552959529999839 ) ) ;
#721 = CARTESIAN_POINT ( 'NONE',  ( -5.101575545643076026, 43.27312978694624945, -136.0552959529885015 ) ) ;
#722 = EDGE_LOOP ( 'NONE', ( #8412, #1698, #20815, #12753, #12822 ) ) ;
#723 = AXIS2_PLACEMENT_3D ( 'NONE', #12821, #5462, #12706 ) ;
#724 = DIRECTION ( 'NONE',  ( 1.000000000000000000, 0.000000000000000000, -2.259525899719999991E-12 ) ) ;
#725 = DIRECTION ( 'NONE',  ( 0.000000000000000000, 1.000000000000000000, 0.000000000000000000 ) ) ;
#726 = ORIENTED_EDGE ( 'NONE', *, *, #17540, .T. ) ;
#727 = ORIENTED_EDGE ( 'NONE', *, *, #8627, .F. ) ;
#728 = CARTESIAN_POINT ( 'NONE',  ( 2.989143058887297588, -0.8786408349372282212, -150.0552959529999839 ) ) ;
#729 = CIRCLE ( 'NONE', #20480, 1.000000000000000888 ) ;
#730 = CARTESIAN_POINT ( 'NONE',  ( 31.50000000000000000, -21.03620104879999886, -136.5552959530000123 ) ) ;
#731 = AXIS2_PLACEMENT_3D ( 'NONE', #8142, #11836, #22803 ) ;
#732 = DIRECTION ( 'NONE',  ( 1.527666881879999979E-13, 8.171241461240000022E-13, 1.000000000000000000 ) ) ;
#733 = CARTESIAN_POINT ( 'NONE',  ( -21.35824191589811605, -3.250000000000000000, -146.3157682190075093 ) ) ;
#734 = ORIENTED_EDGE ( 'NONE', *, *, #17234, .F. ) ;
#735 = CARTESIAN_POINT ( 'NONE',  ( 25.00000852249999994, -26.83294714660000224, -143.5552959529999839 ) ) ;
#736 = CARTESIAN_POINT ( 'NONE',  ( -35.47299999999999898, 14.00000000000000000, -144.0552959529999839 ) ) ;
#737 = EDGE_CURVE ( 'NONE', #2750, #10162, #17272, .T. ) ;
#738 = VECTOR ( 'NONE', #14054, 1000.000000000000000 ) ;
#739 = CYLINDRICAL_SURFACE ( 'NONE', #11687, 1.499999999999999334 ) ;
#740 = CARTESIAN_POINT ( 'NONE',  ( -21.35824191589999899, -32.00000000000000000, -146.3157682190000060 ) ) ;
#741 = EDGE_CURVE ( 'NONE', #598, #16477, #15266, .T. ) ;
#742 = VECTOR ( 'NONE', #894, 1000.000000000000000 ) ;
#743 = CARTESIAN_POINT ( 'NONE',  ( -24.79382848429712638, 38.90154695920348615, -148.2729990965086699 ) ) ;
#744 = EDGE_CURVE ( 'NONE', #22823, #11439, #6921, .T. ) ;
#745 = CARTESIAN_POINT ( 'NONE',  ( -15.70784696974144801, 32.45430872951681778, -144.2620499800023879 ) ) ;
#746 = CARTESIAN_POINT ( 'NONE',  ( -16.93132238861308281, 33.26380838982603194, -143.5428277902702803 ) ) ;
#747 = DIRECTION ( 'NONE',  ( 0.9944529286486341046, -0.1051825684329612265, -4.469111776238355154E-12 ) ) ;
#748 = LINE ( 'NONE', #982, #17937 ) ;
#749 = CARTESIAN_POINT ( 'NONE',  ( 23.40529971389999986, -31.60139774330000151, -148.5552959529999839 ) ) ;
#750 = AXIS2_PLACEMENT_3D ( 'NONE', #14418, #16324, #33 ) ;
#751 = VERTEX_POINT ( 'NONE', #19292 ) ;
#752 = DIRECTION ( 'NONE',  ( 0.000000000000000000, 1.000000000000000000, 0.000000000000000000 ) ) ;
#753 = AXIS2_PLACEMENT_3D ( 'NONE', #701, #11861, #18779 ) ;
#754 = ORIENTED_EDGE ( 'NONE', *, *, #1639, .F. ) ;
#755 = DIRECTION ( 'NONE',  ( -2.257039000139999987E-12, 0.000000000000000000, -1.000000000000000000 ) ) ;
#756 = CIRCLE ( 'NONE', #18597, 2.600000000000000089 ) ;
#757 = CIRCLE ( 'NONE', #2659, 9.999999999999998224 ) ;
#758 = CARTESIAN_POINT ( 'NONE',  ( -22.07763076357180054, 37.06632353693598247, -147.8362371613994242 ) ) ;
#759 = DIRECTION ( 'NONE',  ( -0.000000000000000000, 1.000000000000000000, 0.000000000000000000 ) ) ;
#760 = VERTEX_POINT ( 'NONE', #3003 ) ;
#761 = CARTESIAN_POINT ( 'NONE',  ( -13.64404366366992072, 33.71937897316467314, -142.3027892629986013 ) ) ;
#762 = CARTESIAN_POINT ( 'NONE',  ( 12.50000000010000001, 20.50000000000000000, -147.5552959529999839 ) ) ;
#763 = CARTESIAN_POINT ( 'NONE',  ( 3.175226511974131860, 13.75903940329096287, -150.0552959529999839 ) ) ;
#764 = DIRECTION ( 'NONE',  ( 1.000000000000000000, 0.000000000000000000, 0.000000000000000000 ) ) ;
#765 = CARTESIAN_POINT ( 'NONE',  ( -27.26567793380000282, 36.96940380710000085, -148.4835048639999968 ) ) ;
#766 = LINE ( 'NONE', #643, #16554 ) ;
#767 = CARTESIAN_POINT ( 'NONE',  ( -7.682760800853645655, 38.61178422963649837, -140.5440265716989359 ) ) ;
#768 = EDGE_CURVE ( 'NONE', #11140, #3932, #17506, .T. ) ;
#769 = ORIENTED_EDGE ( 'NONE', *, *, #15215, .F. ) ;
#770 = EDGE_CURVE ( 'NONE', #14651, #10724, #872, .T. ) ;
#771 = VECTOR ( 'NONE', #1393, 1000.000000000000000 ) ;
#772 = AXIS2_PLACEMENT_3D ( 'NONE', #23480, #10382, #3617 ) ;
#773 = DIRECTION ( 'NONE',  ( 1.000000000000000000, 0.000000000000000000, -4.429789868254375404E-12 ) ) ;
#774 =( NAMED_UNIT ( * ) PLANE_ANGLE_UNIT ( ) SI_UNIT ( $, .RADIAN. ) );
#775 = VECTOR ( 'NONE', #2814, 1000.000000000000000 ) ;
#776 = AXIS2_PLACEMENT_3D ( 'NONE', #3674, #5214, #14152 ) ;
#777 = VERTEX_POINT ( 'NONE', #13933 ) ;
#778 = CARTESIAN_POINT ( 'NONE',  ( -14.49707537166952598, 35.20425844453338726, -140.3484218534934485 ) ) ;
#779 = CARTESIAN_POINT ( 'NONE',  ( -9.394775000179999225, 34.25903911019999981, -147.4808749560000081 ) ) ;
#780 = FACE_OUTER_BOUND ( 'NONE', #15265, .T. ) ;
#781 = PRODUCT_DEFINITION ( 'UNKNOWN', '', #11904, #8501 ) ;
#782 = ORIENTED_EDGE ( 'NONE', *, *, #7514, .F. ) ;
#783 = CARTESIAN_POINT ( 'NONE',  ( 19.13369214859999801, 50.50000000000000000, -149.5552959529999839 ) ) ;
#784 = EDGE_CURVE ( 'NONE', #19299, #9007, #13572, .T. ) ;
#785 = CARTESIAN_POINT ( 'NONE',  ( 8.250000000030000891, -37.98606797749999942, -136.0552959530000123 ) ) ;
#786 = ORIENTED_EDGE ( 'NONE', *, *, #16235, .T. ) ;
#787 = CARTESIAN_POINT ( 'NONE',  ( -20.26899604970972035, 40.93030953072783973, -143.7497896408596034 ) ) ;
#788 = CARTESIAN_POINT ( 'NONE',  ( -18.53945141080000170, 39.74065879090000664, -147.6687609889999919 ) ) ;
#789 = AXIS2_PLACEMENT_3D ( 'NONE', #10567, #19991, #14634 ) ;
#790 = CARTESIAN_POINT ( 'NONE',  ( 8.013182962905725404, 38.41915155171203367, -146.1134792699380114 ) ) ;
#791 = VECTOR ( 'NONE', #522, 1000.000000000000000 ) ;
#792 = EDGE_CURVE ( 'NONE', #34, #13141, #18820, .T. ) ;
#793 = DIRECTION ( 'NONE',  ( -2.507771768019999718E-12, -1.592654864069999939E-17, 1.000000000000000000 ) ) ;
#794 = CARTESIAN_POINT ( 'NONE',  ( -24.98993381957792792, 33.76017858760970825, -142.1401211143833621 ) ) ;
#795 = EDGE_LOOP ( 'NONE', ( #318, #13967, #2520, #17759 ) ) ;
#796 = LINE ( 'NONE', #23004, #6121 ) ;
#797 = ORIENTED_EDGE ( 'NONE', *, *, #13969, .F. ) ;
#798 = DIRECTION ( 'NONE',  ( -1.000000000000000000, 0.000000000000000000, 2.258108725280000263E-12 ) ) ;
#799 = ADVANCED_FACE ( 'NONE', ( #15723 ), #13459, .T. ) ;
#800 = ORIENTED_EDGE ( 'NONE', *, *, #6653, .T. ) ;
#801 = CARTESIAN_POINT ( 'NONE',  ( -27.26567793390747596, 36.96940380712532459, -148.4835048638151989 ) ) ;
#802 = VERTEX_POINT ( 'NONE', #11658 ) ;
#803 = DIRECTION ( 'NONE',  ( 8.955190032048950803E-12, -9.104778821523669707E-13, 1.000000000000000000 ) ) ;
#804 = ORIENTED_EDGE ( 'NONE', *, *, #23482, .F. ) ;
#805 = DIRECTION ( 'NONE',  ( -1.000000000000000000, 0.000000000000000000, 2.257423253620000194E-12 ) ) ;
#806 = ORIENTED_EDGE ( 'NONE', *, *, #21641, .F. ) ;
#807 = VECTOR ( 'NONE', #9050, 1000.000000000000227 ) ;
#808 = ORIENTED_EDGE ( 'NONE', *, *, #13766, .F. ) ;
#809 = CARTESIAN_POINT ( 'NONE',  ( 32.50000000000000000, -0.03620104877499999430, -136.0552959530000123 ) ) ;
#810 = EDGE_CURVE ( 'NONE', #5749, #6401, #18935, .T. ) ;
#811 = DIRECTION ( 'NONE',  ( 1.000000000000000000, 0.000000000000000000, -8.953948693601887499E-12 ) ) ;
#812 = CARTESIAN_POINT ( 'NONE',  ( -10.90809651384244461, 40.52503132629866656, -142.2168021453966276 ) ) ;
#813 = CARTESIAN_POINT ( 'NONE',  ( 6.500000000149999124, 20.50000000000000000, -143.5552959529999839 ) ) ;
#814 = CARTESIAN_POINT ( 'NONE',  ( 22.68320006080000084, -24.50000000000000000, -148.5552959529999839 ) ) ;
#815 = CARTESIAN_POINT ( 'NONE',  ( -9.483015687148979467, 40.53201449227000097, -146.0034198470924025 ) ) ;
#816 = ORIENTED_EDGE ( 'NONE', *, *, #7911, .T. ) ;
#817 = DIRECTION ( 'NONE',  ( -0.9968185442904001770, 0.07970438983373183406, 8.881784197001251061E-14 ) ) ;
#818 =( BOUNDED_SURFACE ( )  B_SPLINE_SURFACE ( 5, 5, ( 
 ( #14854, #2244, #20790, #18525, #4481, #22111 ),
 ( #9469, #16623, #20557, #16863, #16745, #5914 ),
 ( #13169, #4131, #5800, #573, #11374, #15078 ),
 ( #6031, #4256, #690, #2591, #6153, #18768 ),
 ( #2479, #4366, #7920, #15202, #15677, #928 ),
 ( #10414, #10302, #6619, #12209, #12321, #19485 ),
 ( #8274, #22940, #17688, #15426, #19230, #6508 ),
 ( #17329, #14123, #20918, #15546, #3181, #2943 ),
 ( #10052, #1396, #8622, #21268, #21033, #15896 ),
 ( #8403, #17577, #8154, #13994, #23161, #4840 ),
 ( #6858, #3069, #21391, #5077, #22685, #1293 ),
 ( #2714, #13881, #21152, #6380, #23048, #9941 ) ),
 .UNSPECIFIED., .F., .F., .F. ) 
 B_SPLINE_SURFACE_WITH_KNOTS ( ( 6, 3, 3, 6 ),
 ( 6, 6 ),
 ( 0.000000000000000000, 4.346865784160000246, 8.778337911509998648, 13.29702284770000098 ),
 ( 1.570796326505564888, 3.141592653590000062 ),
 .UNSPECIFIED. ) 
 GEOMETRIC_REPRESENTATION_ITEM ( )  RATIONAL_B_SPLINE_SURFACE ( (
 ( 0.2500000000000000000, 0.2499999999631480063, 0.2999999999447220400, 0.3999999999262959793, 0.5999999999262960459, 1.000000000000000000),
 ( 0.2500000000000000000, 0.2499999999631480063, 0.2999999999447220400, 0.3999999999262959793, 0.5999999999262960459, 1.000000000000000000),
 ( 0.2500000000000000000, 0.2499999999631480063, 0.2999999999447220400, 0.3999999999262959793, 0.5999999999262960459, 1.000000000000000000),
 ( 0.2500000000000000000, 0.2499999999631480063, 0.2999999999447220400, 0.3999999999262959793, 0.5999999999262960459, 1.000000000000000000),
 ( 0.2500000000000000000, 0.2499999999631480063, 0.2999999999447220400, 0.3999999999262959793, 0.5999999999262960459, 1.000000000000000000),
 ( 0.2500000000000000000, 0.2499999999631480063, 0.2999999999447220400, 0.3999999999262959793, 0.5999999999262960459, 1.000000000000000000),
 ( 0.2500000000000000000, 0.2499999999631480063, 0.2999999999447220400, 0.3999999999262959793, 0.5999999999262960459, 1.000000000000000000),
 ( 0.2500000000000000000, 0.2499999999631480063, 0.2999999999447220400, 0.3999999999262959793, 0.5999999999262960459, 1.000000000000000000),
 ( 0.2500000000000000000, 0.2499999999631480063, 0.2999999999447220400, 0.3999999999262959793, 0.5999999999262960459, 1.000000000000000000),
 ( 0.2500000000000000000, 0.2499999999631480063, 0.2999999999447220400, 0.3999999999262959793, 0.5999999999262960459, 1.000000000000000000),
 ( 0.2500000000000000000, 0.2499999999631480063, 0.2999999999447220400, 0.3999999999262959793, 0.5999999999262960459, 1.000000000000000000),
 ( 0.2500000000000000000, 0.2499999999631480063, 0.2999999999447220400, 0.3999999999262959793, 0.5999999999262960459, 1.000000000000000000) ) ) 
 REPRESENTATION_ITEM ( '' )  SURFACE ( )  );
#819 = EDGE_CURVE ( 'NONE', #5226, #404, #5017, .T. ) ;
#820 = CARTESIAN_POINT ( 'NONE',  ( -14.24884431172416832, 36.97292245485109419, -139.4994906131685184 ) ) ;
#821 = ADVANCED_FACE ( 'NONE', ( #16081 ), #23100, .T. ) ;
#822 = LINE ( 'NONE', #2948, #3 ) ;
#823 = VECTOR ( 'NONE', #20074, 1000.000000000000000 ) ;
#824 = VERTEX_POINT ( 'NONE', #5124 ) ;
#825 = VECTOR ( 'NONE', #18383, 1000.000000000000000 ) ;
#826 = EDGE_CURVE ( 'NONE', #15229, #14150, #20135, .T. ) ;
#827 = ADVANCED_FACE ( 'NONE', ( #6913 ), #21441, .F. ) ;
#828 = CARTESIAN_POINT ( 'NONE',  ( -32.50000000000000000, -24.50000000000000000, -150.0552959529999839 ) ) ;
#829 = DIRECTION ( 'NONE',  ( -2.257144641399999941E-12, 0.000000000000000000, -1.000000000000000000 ) ) ;
#830 = ORIENTED_EDGE ( 'NONE', *, *, #17504, .T. ) ;
#831 = CARTESIAN_POINT ( 'NONE',  ( 11.53320006080000049, -24.50000000000000000, -148.5552959529999839 ) ) ;
#832 = DIRECTION ( 'NONE',  ( -0.1739442350240419932, -0.9847555042252370550, 8.300754441162000146E-13 ) ) ;
#833 = EDGE_LOOP ( 'NONE', ( #16768, #6878, #10888, #18161, #3058, #10823 ) ) ;
#834 = PLANE ( 'NONE',  #6066 ) ;
#835 = CARTESIAN_POINT ( 'NONE',  ( 13.68320006080000084, -19.50000000000000000, -148.5552959529999839 ) ) ;
#836 = ORIENTED_EDGE ( 'NONE', *, *, #936, .F. ) ;
#837 = LINE ( 'NONE', #2962, #359 ) ;
#838 = CARTESIAN_POINT ( 'NONE',  ( -24.90252082140812107, 32.60880315529160356, -143.5690609613828030 ) ) ;
#839 = ORIENTED_EDGE ( 'NONE', *, *, #2461, .T. ) ;
#840 = DIRECTION ( 'NONE',  ( 0.000000000000000000, -1.000000000000000000, -1.592654864069999939E-17 ) ) ;
#841 = ORIENTED_EDGE ( 'NONE', *, *, #2753, .F. ) ;
#842 = CARTESIAN_POINT ( 'NONE',  ( -9.157754307299999397, -15.75963164970000108, -148.5552959529999839 ) ) ;
#843 = CARTESIAN_POINT ( 'NONE',  ( -34.50000000000000000, -35.00000000000000000, -151.0552959529999839 ) ) ;
#844 = VERTEX_POINT ( 'NONE', #14722 ) ;
#845 = VECTOR ( 'NONE', #2349, 1000.000000000000000 ) ;
#846 = DIRECTION ( 'NONE',  ( -0.07970438983373200059, -0.9968185442904001770, 8.268372250843320857E-13 ) ) ;
#847 = AXIS2_PLACEMENT_3D ( 'NONE', #18126, #23365, #1838 ) ;
#848 = AXIS2_PLACEMENT_3D ( 'NONE', #14666, #9179, #20152 ) ;
#849 = EDGE_CURVE ( 'NONE', #8868, #17995, #10312, .T. ) ;
#850 = ORIENTED_EDGE ( 'NONE', *, *, #21643, .T. ) ;
#851 = CARTESIAN_POINT ( 'NONE',  ( -9.999999999959999997, 19.50000000000000000, -136.0552959530000123 ) ) ;
#852 = DIRECTION ( 'NONE',  ( 1.526468026909860048E-13, 8.159623473498529972E-13, 1.000000000000000000 ) ) ;
#853 = ORIENTED_EDGE ( 'NONE', *, *, #17082, .T. ) ;
#854 = EDGE_CURVE ( 'NONE', #14669, #14970, #11031, .T. ) ;
#855 = ORIENTED_EDGE ( 'NONE', *, *, #15175, .F. ) ;
#856 = CARTESIAN_POINT ( 'NONE',  ( 7.683200060759999950, -19.50000000000000000, -148.5552959529999839 ) ) ;
#857 = CARTESIAN_POINT ( 'NONE',  ( -30.60952439866935748, 40.96074107050382906, -145.5181652820941167 ) ) ;
#858 = CARTESIAN_POINT ( 'NONE',  ( -14.11967125442052051, 36.98834135278355717, -140.5455248811183822 ) ) ;
#859 = DIRECTION ( 'NONE',  ( 0.000000000000000000, -1.000000000000000000, 8.159623473500000156E-13 ) ) ;
#860 = ORIENTED_EDGE ( 'NONE', *, *, #19332, .F. ) ;
#861 = CARTESIAN_POINT ( 'NONE',  ( 31.50000000000000000, -33.03620104880000241, -143.0552959529999839 ) ) ;
#862 = VECTOR ( 'NONE', #11868, 1000.000000000000000 ) ;
#863 = AXIS2_PLACEMENT_3D ( 'NONE', #7028, #8562, #12370 ) ;
#864 = CARTESIAN_POINT ( 'NONE',  ( -46.50000000000000000, 37.00000000000000000, -148.4460207619999892 ) ) ;
#865 = VECTOR ( 'NONE', #15700, 1000.000000000000000 ) ;
#866 = DIRECTION ( 'NONE',  ( 0.000000000000000000, 1.093106450072369968E-12, -1.000000000000000000 ) ) ;
#867 = CARTESIAN_POINT ( 'NONE',  ( -7.520331543250000195, 50.50000000000000000, -149.5552959529999839 ) ) ;
#868 = CARTESIAN_POINT ( 'NONE',  ( -24.23404356110848568, 41.65913112518386185, -144.5746520422516994 ) ) ;
#869 = CARTESIAN_POINT ( 'NONE',  ( -16.92867099909999595, 34.38083942290000294, -140.2753207150000208 ) ) ;
#870 = CARTESIAN_POINT ( 'NONE',  ( -16.69209583599786484, 32.46303108206343069, -144.3722252073379764 ) ) ;
#871 = CARTESIAN_POINT ( 'NONE',  ( 20.50000000000000000, 22.50000000000000000, -151.0552959529999839 ) ) ;
#872 = LINE ( 'NONE', #6210, #17180 ) ;
#873 = DIRECTION ( 'NONE',  ( 0.000000000000000000, -1.000000000000000000, 0.000000000000000000 ) ) ;
#874 = ORIENTED_EDGE ( 'NONE', *, *, #177, .T. ) ;
#875 = CARTESIAN_POINT ( 'NONE',  ( -10.09730733349775100, 33.57364382018241855, -143.4697625029285746 ) ) ;
#876 = CARTESIAN_POINT ( 'NONE',  ( -29.36003260551135341, 40.56893091377379079, -146.2070596149844448 ) ) ;
#877 = DIRECTION ( 'NONE',  ( -2.257144641399999941E-12, 8.049635416090000264E-35, -1.000000000000000000 ) ) ;
#878 = ORIENTED_EDGE ( 'NONE', *, *, #3986, .T. ) ;
#879 = CIRCLE ( 'NONE', #6567, 0.5000000000000004441 ) ;
#880 = DIRECTION ( 'NONE',  ( -1.000000000000000000, 5.094701932209999624E-24, 2.257144641399999941E-12 ) ) ;
#881 = EDGE_CURVE ( 'NONE', #17860, #7320, #15289, .T. ) ;
#882 = CARTESIAN_POINT ( 'NONE',  ( -22.09472268147270668, 35.57605554356849353, -147.3183388289436948 ) ) ;
#883 = CARTESIAN_POINT ( 'NONE',  ( 19.68320006079999729, -24.50000000000000000, -149.3052959529999839 ) ) ;
#884 = ORIENTED_EDGE ( 'NONE', *, *, #17515, .F. ) ;
#885 = CARTESIAN_POINT ( 'NONE',  ( -22.68921981444905356, 38.61093386690951945, -140.6331873800498613 ) ) ;
#886 = DIRECTION ( 'NONE',  ( 2.257749542879999954E-12, 0.000000000000000000, 1.000000000000000000 ) ) ;
#887 = LINE ( 'NONE', #1123, #18501 ) ;
#888 = DIRECTION ( 'NONE',  ( -0.9892101392001054760, 0.1465035852930155480, 4.471739159800472250E-12 ) ) ;
#889 = CARTESIAN_POINT ( 'NONE',  ( -9.953901651018769670, 37.05155446198870095, -148.5872971971928962 ) ) ;
#890 = LINE ( 'NONE', #6109, #6665 ) ;
#891 = CARTESIAN_POINT ( 'NONE',  ( -8.547556706628435919, 40.01242579642496366, -142.2846414162569317 ) ) ;
#892 = ORIENTED_EDGE ( 'NONE', *, *, #13892, .T. ) ;
#893 = PRESENTATION_LAYER_ASSIGNMENT (  '', '', ( #17210 ) ) ;
#894 = DIRECTION ( 'NONE',  ( 1.000000000000000000, 0.000000000000000000, 0.000000000000000000 ) ) ;
#895 = FILL_AREA_STYLE ('',( #4447 ) ) ;
#896 = VERTEX_POINT ( 'NONE', #3343 ) ;
#897 = DIRECTION ( 'NONE',  ( -1.000000000000000000, 5.094701932209999624E-24, 2.257144641399999941E-12 ) ) ;
#898 = CARTESIAN_POINT ( 'NONE',  ( -4.499999999929999994, 41.25000000000000000, -138.0552959530000123 ) ) ;
#899 = FACE_OUTER_BOUND ( 'NONE', #6411, .T. ) ;
#900 = ORIENTED_EDGE ( 'NONE', *, *, #13310, .T. ) ;
#901 = CARTESIAN_POINT ( 'NONE',  ( 0.5000000001500000124, 16.89444872450000190, -143.5552959529999839 ) ) ;
#902 = LINE ( 'NONE', #9909, #21670 ) ;
#903 = VERTEX_POINT ( 'NONE', #1455 ) ;
#904 = DIRECTION ( 'NONE',  ( 0.000000000000000000, -2.257144641399999941E-12, -1.000000000000000000 ) ) ;
#905 = EDGE_CURVE ( 'NONE', #11614, #16880, #2022, .T. ) ;
#906 = CARTESIAN_POINT ( 'NONE',  ( -18.36556700629002492, 41.35841174322762015, -144.3779443069900026 ) ) ;
#907 = EDGE_CURVE ( 'NONE', #3556, #4774, #9244, .T. ) ;
#908 = CARTESIAN_POINT ( 'NONE',  ( 7.138086557144586841, 37.63063951478724078, -146.4749235844574002 ) ) ;
#909 = DIRECTION ( 'NONE',  ( 0.000000000000000000, 0.000000000000000000, 1.000000000000000000 ) ) ;
#910 = VECTOR ( 'NONE', #8859, 1000.000000000000000 ) ;
#911 = CARTESIAN_POINT ( 'NONE',  ( -24.30183382816920812, 35.51482525056968598, -147.3052200786065669 ) ) ;
#912 = LINE ( 'NONE', #16633, #6713 ) ;
#913 = ORIENTED_EDGE ( 'NONE', *, *, #20692, .F. ) ;
#914 = CARTESIAN_POINT ( 'NONE',  ( 24.11847952820000174, -31.58456057200000089, -143.0552959529999839 ) ) ;
#915 = VERTEX_POINT ( 'NONE', #10353 ) ;
#916 = SURFACE_SIDE_STYLE ('',( #15534 ) ) ;
#917 = ORIENTED_EDGE ( 'NONE', *, *, #16657, .T. ) ;
#918 = DIRECTION ( 'NONE',  ( 0.000000000000000000, 1.000000000000000000, 0.000000000000000000 ) ) ;
#919 = VERTEX_POINT ( 'NONE', #10579 ) ;
#920 = LINE ( 'NONE', #8145, #8728 ) ;
#921 = ORIENTED_EDGE ( 'NONE', *, *, #10976, .T. ) ;
#922 = ORIENTED_EDGE ( 'NONE', *, *, #6201, .F. ) ;
#923 = AXIS2_PLACEMENT_3D ( 'NONE', #3964, #20620, #5970 ) ;
#924 = PLANE ( 'NONE',  #10610 ) ;
#925 = CARTESIAN_POINT ( 'NONE',  ( -32.50000000000000000, 76.00000000000000000, -132.5552959530000123 ) ) ;
#926 = DIRECTION ( 'NONE',  ( 1.000000000000000000, 0.000000000000000000, 0.000000000000000000 ) ) ;
#927 = CARTESIAN_POINT ( 'NONE',  ( -33.50000000000000000, -35.00000000000000000, -151.0552959529999839 ) ) ;
#928 = CARTESIAN_POINT ( 'NONE',  ( -6.518232409689999507, 33.41592120480000006, -146.1606736330000160 ) ) ;
#929 = DIRECTION ( 'NONE',  ( 0.9957290851625899553, -0.09232328504376198508, -9.001390970786290700E-12 ) ) ;
#930 = ORIENTED_EDGE ( 'NONE', *, *, #18567, .F. ) ;
#931 = DIRECTION ( 'NONE',  ( 1.000000000000000000, 0.000000000000000000, -2.257453483404485639E-12 ) ) ;
#932 = CARTESIAN_POINT ( 'NONE',  ( 9.900763825459462097, 37.53873760029328821, -146.4970002627086956 ) ) ;
#933 = CARTESIAN_POINT ( 'NONE',  ( -9.971101149720000834, 37.05360750090000721, -147.8421425029999909 ) ) ;
#934 = ORIENTED_EDGE ( 'NONE', *, *, #10109, .T. ) ;
#935 = VECTOR ( 'NONE', #3004, 1000.000000000000000 ) ;
#936 = EDGE_CURVE ( 'NONE', #19018, #10871, #218, .T. ) ;
#937 = CARTESIAN_POINT ( 'NONE',  ( -17.71320442848650956, 38.77266098830207142, -148.1578736811549959 ) ) ;
#938 = DIRECTION ( 'NONE',  ( 2.257144641399999941E-12, 0.000000000000000000, 1.000000000000000000 ) ) ;
#939 = EDGE_LOOP ( 'NONE', ( #4957, #18808, #12429, #12764 ) ) ;
#940 = FACE_OUTER_BOUND ( 'NONE', #11497, .T. ) ;
#941 = VERTEX_POINT ( 'NONE', #11143 ) ;
#942 = CARTESIAN_POINT ( 'NONE',  ( 4.999999999879999990, -1.500000000000000000, -135.4552959529999896 ) ) ;
#943 = FACE_OUTER_BOUND ( 'NONE', #18495, .T. ) ;
#944 = ORIENTED_EDGE ( 'NONE', *, *, #2669, .F. ) ;
#945 = CARTESIAN_POINT ( 'NONE',  ( -14.80303414763277914, 37.74518406597707099, -140.0709723763587249 ) ) ;
#946 = CARTESIAN_POINT ( 'NONE',  ( -26.23154108612487789, 35.99110338347298921, -139.4510183337245621 ) ) ;
#947 = VERTEX_POINT ( 'NONE', #8804 ) ;
#948 = EDGE_CURVE ( 'NONE', #8156, #9207, #7576, .T. ) ;
#949 = DIRECTION ( 'NONE',  ( -3.552713678800000397E-15, 0.000000000000000000, 1.000000000000000000 ) ) ;
#950 = EDGE_LOOP ( 'NONE', ( #4953, #19405, #13964, #10896 ) ) ;
#951 = CARTESIAN_POINT ( 'NONE',  ( 3.611688725869999975E-11, -51.50000000000000000, -136.0552959530000123 ) ) ;
#952 = EDGE_CURVE ( 'NONE', #22710, #537, #20436, .T. ) ;
#953 = DIRECTION ( 'NONE',  ( 1.000000000000000000, 0.000000000000000000, 0.000000000000000000 ) ) ;
#954 = VERTEX_POINT ( 'NONE', #20786 ) ;
#955 = CARTESIAN_POINT ( 'NONE',  ( 2.218297500559999857, -15.44723318490000175, -146.5552959529999839 ) ) ;
#956 = EDGE_CURVE ( 'NONE', #22736, #2628, #6149, .T. ) ;
#957 = ORIENTED_EDGE ( 'NONE', *, *, #4177, .T. ) ;
#958 = FACE_BOUND ( 'NONE', #19822, .T. ) ;
#959 = EDGE_CURVE ( 'NONE', #19705, #16855, #22573, .T. ) ;
#960 = CARTESIAN_POINT ( 'NONE',  ( 1.829659965300000080, -16.02499107890000118, -143.5552959529999839 ) ) ;
#961 = AXIS2_PLACEMENT_3D ( 'NONE', #19818, #21604, #5064 ) ;
#962 = ORIENTED_EDGE ( 'NONE', *, *, #13286, .T. ) ;
#963 = VERTEX_POINT ( 'NONE', #16860 ) ;
#964 = CARTESIAN_POINT ( 'NONE',  ( 7.121359165062772334, -1.989143058887300475, -150.0552959530000123 ) ) ;
#965 = LINE ( 'NONE', #22723, #3243 ) ;
#966 = LINE ( 'NONE', #6082, #22322 ) ;
#967 = DIRECTION ( 'NONE',  ( 1.000000000000000000, 0.000000000000000000, 0.000000000000000000 ) ) ;
#968 = VERTEX_POINT ( 'NONE', #16742 ) ;
#969 = DIRECTION ( 'NONE',  ( -1.000000000000000000, -2.602084704489999637E-17, 1.701177084830000066E-20 ) ) ;
#970 = DIRECTION ( 'NONE',  ( 0.000000000000000000, 0.000000000000000000, 1.000000000000000000 ) ) ;
#971 = LINE ( 'NONE', #21197, #17113 ) ;
#972 = CARTESIAN_POINT ( 'NONE',  ( -13.50000000000000000, -42.80126216859517996, -150.0552959529999839 ) ) ;
#973 = CARTESIAN_POINT ( 'NONE',  ( -25.35824191589811960, -34.50000000000000000, -146.3157682190081346 ) ) ;
#974 = DIRECTION ( 'NONE',  ( -1.000000000000000000, 0.000000000000000000, -2.273736754430000208E-12 ) ) ;
#975 = VECTOR ( 'NONE', #19311, 1000.000000000000114 ) ;
#976 = ORIENTED_EDGE ( 'NONE', *, *, #17520, .F. ) ;
#977 = DIRECTION ( 'NONE',  ( 0.000000000000000000, 1.000000000000000000, 0.000000000000000000 ) ) ;
#978 = EDGE_CURVE ( 'NONE', #17690, #8147, #22334, .T. ) ;
#979 = CARTESIAN_POINT ( 'NONE',  ( -16.20147620251679754, 33.40528963976247923, -143.4816615022228063 ) ) ;
#980 = EDGE_CURVE ( 'NONE', #11681, #2055, #20670, .T. ) ;
#981 = DIRECTION ( 'NONE',  ( 0.000000000000000000, 0.000000000000000000, -1.000000000000000000 ) ) ;
#982 = CARTESIAN_POINT ( 'NONE',  ( -31.75000000000000000, 19.50000000000000000, -151.0552959529999839 ) ) ;
#983 = DIRECTION ( 'NONE',  ( -0.1185248058630065937, 0.9929510916430560608, 2.679939603570147632E-13 ) ) ;
#984 = EDGE_CURVE ( 'NONE', #1160, #14539, #11488, .T. ) ;
#985 = ORIENTED_EDGE ( 'NONE', *, *, #18589, .F. ) ;
#986 = CARTESIAN_POINT ( 'NONE',  ( -9.685596112079144504, 34.85788159552594578, -146.7686248962264983 ) ) ;
#987 = DIRECTION ( 'NONE',  ( 0.000000000000000000, 1.093106450072369968E-12, -1.000000000000000000 ) ) ;
#988 = APPLICATION_CONTEXT ( 'automotive_design' ) ;
#989 = CARTESIAN_POINT ( 'NONE',  ( -24.97797643630000053, 37.05442817780000553, -147.8575004449999994 ) ) ;
#990 = VERTEX_POINT ( 'NONE', #9815 ) ;
#991 = CARTESIAN_POINT ( 'NONE',  ( -32.50000000000000000, 51.50000000000000000, -137.0552959530000123 ) ) ;
#993 = CARTESIAN_POINT ( 'NONE',  ( -28.80902675595255857, 36.08666534566612683, -139.5659208846137744 ) ) ;
#992 = AXIS2_PLACEMENT_3D ( 'NONE', #3546, #17821, #18174 ) ;
#994 = AXIS2_PLACEMENT_3D ( 'NONE', #15653, #1375, #10392 ) ;
#995 = DIRECTION ( 'NONE',  ( 0.000000000000000000, 1.000000000000000000, 0.000000000000000000 ) ) ;
#996 = ORIENTED_EDGE ( 'NONE', *, *, #10115, .F. ) ;
#997 = CARTESIAN_POINT ( 'NONE',  ( -13.92432874550000044, 37.01165864720000087, -139.5650670249999905 ) ) ;
#998 = CARTESIAN_POINT ( 'NONE',  ( 24.75935218339999722, -28.32938697159999819, -147.5552959529999839 ) ) ;
#999 = DIRECTION ( 'NONE',  ( 1.000000000000000000, 0.000000000000000000, -2.256131789327549967E-12 ) ) ;
#1000 = CARTESIAN_POINT ( 'NONE',  ( 6.750000000000000000, -36.00000000000000000, -150.0552959529999839 ) ) ;
#1001 = CARTESIAN_POINT ( 'NONE',  ( -9.897232795978197828, 34.02093318812835321, -147.8794181089841118 ) ) ;
#1002 = PLANE ( 'NONE',  #9686 ) ;
#1003 = CARTESIAN_POINT ( 'NONE',  ( 8.701166446538422861, -33.70126136998415944, -150.0552959529999839 ) ) ;
#1004 = ORIENTED_EDGE ( 'NONE', *, *, #5617, .T. ) ;
#1005 =( NAMED_UNIT ( * ) PLANE_ANGLE_UNIT ( ) SI_UNIT ( $, .RADIAN. ) );
#1006 = EDGE_CURVE ( 'NONE', #990, #7716, #8150, .T. ) ;
#1007 = EDGE_CURVE ( 'NONE', #5202, #6635, #17208, .T. ) ;
#1008 = ORIENTED_EDGE ( 'NONE', *, *, #12992, .F. ) ;
#1009 = PRODUCT_DEFINITION_SHAPE ( 'NONE', 'NONE',  #23547 ) ;
#1010 = VECTOR ( 'NONE', #18945, 1000.000000000000000 ) ;
#1011 = CARTESIAN_POINT ( 'NONE',  ( -6.990747311370722805, 33.54994435292839938, -144.4888610368732600 ) ) ;
#1012 = CARTESIAN_POINT ( 'NONE',  ( 32.14594224169999848, -40.79958733389999992, -136.0552959530000123 ) ) ;
#1013 = VECTOR ( 'NONE', #17401, 1000.000000000000000 ) ;
#1014 = FACE_OUTER_BOUND ( 'NONE', #19027, .T. ) ;
#1015 = VERTEX_POINT ( 'NONE', #9697 ) ;
#1016 = DIRECTION ( 'NONE',  ( 0.7071067811865475727, -0.7071067811865475727, -1.595020412044807153E-12 ) ) ;
#1017 = DIRECTION ( 'NONE',  ( -1.000000000000000000, 0.000000000000000000, 0.000000000000000000 ) ) ;
#1018 = ORIENTED_EDGE ( 'NONE', *, *, #17842, .T. ) ;
#1019 = CARTESIAN_POINT ( 'NONE',  ( 5.276897646250000129, -21.39828525539999760, -145.5552959529999839 ) ) ;
#1020 = CARTESIAN_POINT ( 'NONE',  ( -18.46720449282527454, 40.97819876959629681, -144.3328547432334119 ) ) ;
#1021 = DIRECTION ( 'NONE',  ( 0.000000000000000000, -1.000000000000000000, 0.000000000000000000 ) ) ;
#1022 = FACE_OUTER_BOUND ( 'NONE', #1478, .T. ) ;
#1023 = LINE ( 'NONE', #8251, #17696 ) ;
#1024 = AXIS2_PLACEMENT_3D ( 'NONE', #1323, #8898, #21306 ) ;
#1025 = CARTESIAN_POINT ( 'NONE',  ( -24.57863953957676273, 33.12365565967444070, -146.2648171790582126 ) ) ;
#1026 = LINE ( 'NONE', #6599, #12411 ) ;
#1027 = ORIENTED_EDGE ( 'NONE', *, *, #68, .F. ) ;
#1028 = CARTESIAN_POINT ( 'NONE',  ( 6.500000000159999125, 12.50000000000000000, -140.5552959529999839 ) ) ;
#1029 = EDGE_CURVE ( 'NONE', #14361, #2146, #5314, .T. ) ;
#1030 = VERTEX_POINT ( 'NONE', #22453 ) ;
#1031 = CARTESIAN_POINT ( 'NONE',  ( -7.499999999959999997, -2.273736754430000208E-12, -136.0552959530000123 ) ) ;
#1032 = ORIENTED_EDGE ( 'NONE', *, *, #12890, .T. ) ;
#1033 = ADVANCED_FACE ( 'NONE', ( #8037 ), #11249, .T. ) ;
#1034 = CARTESIAN_POINT ( 'NONE',  ( 22.50000000000000000, 39.50000000000000000, -137.0552959530000123 ) ) ;
#1035 = ORIENTED_EDGE ( 'NONE', *, *, #2912, .F. ) ;
#1036 = CARTESIAN_POINT ( 'NONE',  ( -0.2409605966616616968, 23.82477348803141837, -136.0552959529995007 ) ) ;
#1037 = EDGE_CURVE ( 'NONE', #9207, #2750, #18595, .T. ) ;
#1038 = VERTEX_POINT ( 'NONE', #11600 ) ;
#1039 = VECTOR ( 'NONE', #23463, 1000.000000000000000 ) ;
#1040 = ORIENTED_EDGE ( 'NONE', *, *, #20103, .F. ) ;
#1041 = CARTESIAN_POINT ( 'NONE',  ( -4.499999999939999995, 37.00000000000000000, -144.0552959529999839 ) ) ;
#1042 = LINE ( 'NONE', #15781, #17871 ) ;
#1043 = CARTESIAN_POINT ( 'NONE',  ( -5.316799939240000938, 0.9999999999989999111, -150.0552959529999839 ) ) ;
#1044 = CARTESIAN_POINT ( 'NONE',  ( -22.10824191589999899, -4.000000000000000000, -146.3157682190000060 ) ) ;
#1045 = LINE ( 'NONE', #22814, #19399 ) ;
#1046 = CARTESIAN_POINT ( 'NONE',  ( -9.172004967711496093, 41.72460712644299008, -144.4785182484624784 ) ) ;
#1047 = ORIENTED_EDGE ( 'NONE', *, *, #7201, .T. ) ;
#1048 = DIRECTION ( 'NONE',  ( -1.000000000000000000, 0.000000000000000000, 0.000000000000000000 ) ) ;
#1049 = DIRECTION ( 'NONE',  ( 1.526468026909999897E-13, 8.159623473500000156E-13, 1.000000000000000000 ) ) ;
#1050 = CYLINDRICAL_SURFACE ( 'NONE', #8335, 0.7500000000000006661 ) ;
#1051 = ORIENTED_EDGE ( 'NONE', *, *, #16098, .F. ) ;
#1052 = CIRCLE ( 'NONE', #17006, 15.00000000000000000 ) ;
#1053 = DIRECTION ( 'NONE',  ( 1.457985068979999943E-12, -1.723073263340000007E-12, -1.000000000000000000 ) ) ;
#1054 = DIRECTION ( 'NONE',  ( 1.000000000000000000, -5.094701932209999624E-24, -2.257144641399999941E-12 ) ) ;
#1055 = CIRCLE ( 'NONE', #14350, 1.499999999999999556 ) ;
#1056 = ORIENTED_EDGE ( 'NONE', *, *, #18194, .T. ) ;
#1057 = CYLINDRICAL_SURFACE ( 'NONE', #12060, 1.000000000000000888 ) ;
#1058 = DIRECTION ( 'NONE',  ( 0.09232328504376198508, 0.9957290851625899553, 7.981674670826710110E-14 ) ) ;
#1059 = ORIENTED_EDGE ( 'NONE', *, *, #17973, .F. ) ;
#1060 = DIRECTION ( 'NONE',  ( 1.000000000000000000, 1.387778780779999841E-17, 2.506439500389999993E-12 ) ) ;
#1061 = FACE_OUTER_BOUND ( 'NONE', #22766, .T. ) ;
#1062 = VERTEX_POINT ( 'NONE', #22221 ) ;
#1063 = CARTESIAN_POINT ( 'NONE',  ( -14.58163105942842641, 36.93319896293559168, -139.6872257168839440 ) ) ;
#1064 = CARTESIAN_POINT ( 'NONE',  ( -24.79371418826683993, 32.62011804915596258, -144.5039952333266058 ) ) ;
#1065 = EDGE_CURVE ( 'NONE', #12475, #2580, #7691, .T. ) ;
#1066 = EDGE_LOOP ( 'NONE', ( #14610, #17073, #1898, #21878, #8834 ) ) ;
#1067 = PRESENTATION_STYLE_ASSIGNMENT (( #2966 ) ) ;
#1068 = PLANE ( 'NONE',  #6979 ) ;
#1069 = VERTEX_POINT ( 'NONE', #925 ) ;
#1070 = LINE ( 'NONE', #15577, #9079 ) ;
#1071 = CARTESIAN_POINT ( 'NONE',  ( -7.500000000000000000, 19.50000000000000000, -151.0552959529999839 ) ) ;
#1072 = ORIENTED_EDGE ( 'NONE', *, *, #2514, .T. ) ;
#1073 = CARTESIAN_POINT ( 'NONE',  ( -20.60824191589811605, -4.000000000000000000, -146.3157682190056335 ) ) ;
#1075 = AXIS2_PLACEMENT_3D ( 'NONE', #18241, #14778, #157 ) ;
#1074 = PRODUCT_DEFINITION ( 'UNKNOWN', '', #13416, #3518 ) ;
#1076 = ORIENTED_EDGE ( 'NONE', *, *, #1211, .T. ) ;
#1077 = DIRECTION ( 'NONE',  ( -0.7633862853691523176, -0.6459422414661291079, 0.000000000000000000 ) ) ;
#1078 = ADVANCED_FACE ( 'NONE', ( #18650 ), #15316, .F. ) ;
#1079 = VECTOR ( 'NONE', #4853, 1000.000000000000000 ) ;
#1080 = DIRECTION ( 'NONE',  ( 1.000000000000000000, -1.190078432789999897E-50, -2.257144641399999941E-12 ) ) ;
#1081 = ORIENTED_EDGE ( 'NONE', *, *, #17981, .F. ) ;
#1082 = ORIENTED_EDGE ( 'NONE', *, *, #12807, .T. ) ;
#1083 = CARTESIAN_POINT ( 'NONE',  ( -25.35824191590000254, -18.00000000000000000, -144.8157682190000060 ) ) ;
#1084 = EDGE_CURVE ( 'NONE', #13908, #20921, #22689, .T. ) ;
#1085 = PLANE ( 'NONE',  #7781 ) ;
#1086 = FACE_OUTER_BOUND ( 'NONE', #5557, .T. ) ;
#1087 = LINE ( 'NONE', #2519, #375 ) ;
#1088 = EDGE_LOOP ( 'NONE', ( #10214, #10164, #17790, #19615 ) ) ;
#1089 = CARTESIAN_POINT ( 'NONE',  ( -16.30994315220291213, -42.24256961503859031, -136.0552959529631778 ) ) ;
#1090 = CARTESIAN_POINT ( 'NONE',  ( -8.734077015120000453, -11.22642389220000148, -146.5552959529999839 ) ) ;
#1091 = VECTOR ( 'NONE', #21185, 1000.000000000000000 ) ;
#1092 = CARTESIAN_POINT ( 'NONE',  ( 4.499999999879999102, -4.000000000000000000, -132.3031539049999878 ) ) ;
#1093 = CARTESIAN_POINT ( 'NONE',  ( -5.758148842640000709, -13.22138763369999914, -148.5552959529999839 ) ) ;
#1094 = CARTESIAN_POINT ( 'NONE',  ( 15.10199673425556455, 39.50000000000002842, -136.0552959530340615 ) ) ;
#1095 = CARTESIAN_POINT ( 'NONE',  ( 1.354168148130000082, -20.95195702430000040, -143.5552959529999839 ) ) ;
#1096 = VECTOR ( 'NONE', #10422, 1000.000000000000000 ) ;
#1097 = EDGE_CURVE ( 'NONE', #6873, #213, #22682, .T. ) ;
#1098 = ORIENTED_EDGE ( 'NONE', *, *, #3445, .F. ) ;
#1099 = CARTESIAN_POINT ( 'NONE',  ( -15.66251200267681831, 32.89188227335794323, -143.3406170289139254 ) ) ;
#1100 = CARTESIAN_POINT ( 'NONE',  ( 14.50000000010000001, 37.00000000000000000, -144.0552959529999839 ) ) ;
#1101 = DIRECTION ( 'NONE',  ( 1.526468026909999897E-13, 8.159623473500000156E-13, 1.000000000000000000 ) ) ;
#1102 = DIRECTION ( 'NONE',  ( 0.000000000000000000, -1.000000000000000000, 2.273736754430000208E-12 ) ) ;
#1103 = LINE ( 'NONE', #6560, #18040 ) ;
#1104 = VERTEX_POINT ( 'NONE', #12318 ) ;
#1105 = CARTESIAN_POINT ( 'NONE',  ( 9.683200060759999062, -20.50000000000000000, -148.5552959529999839 ) ) ;
#1106 = DIRECTION ( 'NONE',  ( -0.06298685227120542907, -0.9980143568310855251, 1.515824502950130739E-13 ) ) ;
#1107 = EDGE_CURVE ( 'NONE', #9556, #20751, #13681, .T. ) ;
#1108 = FACE_OUTER_BOUND ( 'NONE', #16737, .T. ) ;
#1109 = EDGE_LOOP ( 'NONE', ( #4239, #8656, #12056, #15119 ) ) ;
#1110 = EDGE_CURVE ( 'NONE', #2371, #10397, #1593, .T. ) ;
#1111 = DIRECTION ( 'NONE',  ( -2.257144641399999941E-12, 8.049635416090000264E-35, -1.000000000000000000 ) ) ;
#1112 = VECTOR ( 'NONE', #3564, 1000.000000000000000 ) ;
#1113 = VECTOR ( 'NONE', #12362, 1000.000000000000000 ) ;
#1114 = CARTESIAN_POINT ( 'NONE',  ( -29.10972917886757116, 33.01395076712321952, -141.7686278616081950 ) ) ;
#1115 = DIRECTION ( 'NONE',  ( 2.257157423930000049E-12, 0.000000000000000000, 1.000000000000000000 ) ) ;
#1116 = VERTEX_POINT ( 'NONE', #19482 ) ;
#1117 = AXIS2_PLACEMENT_3D ( 'NONE', #140, #20122, #19888 ) ;
#1118 = CARTESIAN_POINT ( 'NONE',  ( -13.30230152915278197, 36.27094684673078717, -140.3343369752782621 ) ) ;
#1119 = EDGE_CURVE ( 'NONE', #11281, #5200, #3287, .T. ) ;
#1120 = DIRECTION ( 'NONE',  ( 2.257144641399999941E-12, -4.009147065140000298E-51, 1.000000000000000000 ) ) ;
#1121 = VECTOR ( 'NONE', #19395, 1000.000000000000000 ) ;
#1122 = EDGE_CURVE ( 'NONE', #14150, #6123, #4001, .T. ) ;
#1123 = CARTESIAN_POINT ( 'NONE',  ( 29.68320006080000084, 0.9999999999989999111, -149.3052959529999839 ) ) ;
#1124 = CARTESIAN_POINT ( 'NONE',  ( 8.450744908290142021, 38.50000000000001421, -142.0552959529998702 ) ) ;
#1125 = CARTESIAN_POINT ( 'NONE',  ( -9.667609713899818047, 35.97527138268016245, -148.7282639817501035 ) ) ;
#1126 = DIRECTION ( 'NONE',  ( 0.000000000000000000, 1.000000000000000000, 0.000000000000000000 ) ) ;
#1127 = EDGE_CURVE ( 'NONE', #7397, #7971, #1042, .T. ) ;
#1128 = CARTESIAN_POINT ( 'NONE',  ( 4.055709778248144382, -34.64604587945159864, -150.0552959529999839 ) ) ;
#1129 = ADVANCED_FACE ( 'NONE', ( #19115 ), #12963, .F. ) ;
#1130 = ORIENTED_EDGE ( 'NONE', *, *, #23377, .T. ) ;
#1131 = DIRECTION ( 'NONE',  ( 2.257144641399999941E-12, -8.049635416090000264E-35, 1.000000000000000000 ) ) ;
#1132 = AXIS2_PLACEMENT_3D ( 'NONE', #9763, #13584, #4554 ) ;
#1133 = FILL_AREA_STYLE ('',( #8586 ) ) ;
#1134 = CIRCLE ( 'NONE', #9463, 3.000000000000000000 ) ;
#1135 = ORIENTED_EDGE ( 'NONE', *, *, #2562, .F. ) ;
#1136 = CARTESIAN_POINT ( 'NONE',  ( -6.728963506639928482, 33.26001575821830158, -144.4977132839956653 ) ) ;
#1137 = DIRECTION ( 'NONE',  ( 4.518783361002970486E-12, 0.000000000000000000, 1.000000000000000000 ) ) ;
#1138 = FACE_OUTER_BOUND ( 'NONE', #8262, .T. ) ;
#1139 = VECTOR ( 'NONE', #23042, 1000.000000000000000 ) ;
#1140 = VERTEX_POINT ( 'NONE', #21622 ) ;
#1141 = VECTOR ( 'NONE', #22229, 1000.000000000000000 ) ;
#1142 = FACE_OUTER_BOUND ( 'NONE', #8260, .T. ) ;
#1143 = CARTESIAN_POINT ( 'NONE',  ( 7.558347240399999833, -12.62842008530000015, -148.5552959529999839 ) ) ;
#1144 = ORIENTED_EDGE ( 'NONE', *, *, #8369, .T. ) ;
#1145 = FACE_OUTER_BOUND ( 'NONE', #17569, .T. ) ;
#1146 = CARTESIAN_POINT ( 'NONE',  ( -17.68978131337266291, 36.92028947728029920, -140.0842674916291628 ) ) ;
#1147 = CARTESIAN_POINT ( 'NONE',  ( -12.37864083493722589, -41.48914305888730070, -150.0552959530000123 ) ) ;
#1148 = CARTESIAN_POINT ( 'NONE',  ( 7.310213413902445723, 37.91900551518246232, -146.3817958922534217 ) ) ;
#1149 = AXIS2_PLACEMENT_3D ( 'NONE', #23405, #16268, #10529 ) ;
#1150 = DIRECTION ( 'NONE',  ( 2.257144641397284947E-12, -2.714590281723094849E-24, 1.000000000000000000 ) ) ;
#1151 = EDGE_CURVE ( 'NONE', #8640, #1276, #4942, .T. ) ;
#1152 = CARTESIAN_POINT ( 'NONE',  ( -24.16551117144435779, 36.07182940189623821, -148.2420083174796162 ) ) ;
#1153 = CARTESIAN_POINT ( 'NONE',  ( -9.434278515689999978, -18.41834002140000237, -146.5552959529999839 ) ) ;
#1154 = AXIS2_PLACEMENT_3D ( 'NONE', #17896, #14566, #16350 ) ;
#1155 = CARTESIAN_POINT ( 'NONE',  ( -11.75883488016316214, 37.77601231981555685, -140.0882460024616876 ) ) ;
#1156 = VECTOR ( 'NONE', #20344, 1000.000000000000000 ) ;
#1157 = AXIS2_PLACEMENT_3D ( 'NONE', #117, #1784, #12704 ) ;
#1158 = ORIENTED_EDGE ( 'NONE', *, *, #16087, .F. ) ;
#1159 = DIRECTION ( 'NONE',  ( 0.4794255386042040601, 0.8775825618903723147, 0.000000000000000000 ) ) ;
#1160 = VERTEX_POINT ( 'NONE', #8975 ) ;
#1161 = DIRECTION ( 'NONE',  ( 1.000000000000000000, 0.000000000000000000, 0.000000000000000000 ) ) ;
#1162 = VERTEX_POINT ( 'NONE', #16258 ) ;
#1163 = DIRECTION ( 'NONE',  ( 2.257144641399999941E-12, -4.009147065140000298E-51, 1.000000000000000000 ) ) ;
#1164 = EDGE_LOOP ( 'NONE', ( #6286, #1314, #2583, #12664 ) ) ;
#1165 = CARTESIAN_POINT ( 'NONE',  ( 0.5374248537463910402, 25.07581004119176171, -136.0552959530012060 ) ) ;
#1166 = DIRECTION ( 'NONE',  ( 0.9990052710704846461, -0.04459224566432164194, -1.160036675700561719E-13 ) ) ;
#1167 = ORIENTED_EDGE ( 'NONE', *, *, #17932, .F. ) ;
#1168 = VERTEX_POINT ( 'NONE', #23513 ) ;
#1169 = CARTESIAN_POINT ( 'NONE',  ( 21.79964646190000011, -30.87346604779999737, -144.5552959529999839 ) ) ;
#1170 = CARTESIAN_POINT ( 'NONE',  ( -19.14899212252498728, 37.07484167171551093, -147.8220480108043375 ) ) ;
#1171 = FACE_OUTER_BOUND ( 'NONE', #10638, .T. ) ;
#1172 = SURFACE_SIDE_STYLE ('',( #22576 ) ) ;
#1173 = AXIS2_PLACEMENT_3D ( 'NONE', #8912, #5236, #3339 ) ;
#1174 =( BOUNDED_SURFACE ( )  B_SPLINE_SURFACE ( 5, 5, ( 
 ( #6524, #10195, #17596, #1063, #13791, #11624 ),
 ( #3087, #6399, #945, #22834, #18898, #8059 ),
 ( #19022, #2841, #15444, #6639, #20936, #17119 ),
 ( #22594, #23067, #8423, #21171, #6752, #21054 ),
 ( #13538, #11870, #17349, #13660, #20810, #22706 ),
 ( #4501, #11741, #2734, #9961, #17232, #17470 ),
 ( #15693, #10071, #22955, #4859, #12104, #19381 ),
 ( #10321, #10543, #21764, #12454, #12336, #4980 ),
 ( #19733, #10665, #21408, #14256, #7234, #12227 ),
 ( #5450, #15916, #3428, #1418, #18062, #3196 ),
 ( #14499, #12696, #19852, #16162, #23301, #10899 ),
 ( #19502, #16398, #8995, #16042, #19613, #1660 ) ),
 .UNSPECIFIED., .F., .F., .F. ) 
 B_SPLINE_SURFACE_WITH_KNOTS ( ( 6, 3, 3, 6 ),
 ( 6, 6 ),
 ( 0.000000000000000000, 4.151671928079999851, 8.316542232069998875, 12.50501063799999990 ),
 ( 1.570796326769924978, 3.141592653590000062 ),
 .UNSPECIFIED. ) 
 GEOMETRIC_REPRESENTATION_ITEM ( )  RATIONAL_B_SPLINE_SURFACE ( (
 ( 0.2500000000000000000, 0.2499999999968069986, 0.2999999999952105423, 0.3999999999936145190, 0.5999999999936139750, 1.000000000000000000),
 ( 0.2500000000000000000, 0.2499999999968069986, 0.2999999999952105423, 0.3999999999936145190, 0.5999999999936139750, 1.000000000000000000),
 ( 0.2500000000000000000, 0.2499999999968069986, 0.2999999999952105423, 0.3999999999936145190, 0.5999999999936139750, 1.000000000000000000),
 ( 0.2500000000000000000, 0.2499999999968069986, 0.2999999999952105423, 0.3999999999936145190, 0.5999999999936139750, 1.000000000000000000),
 ( 0.2500000000000000000, 0.2499999999968069986, 0.2999999999952105423, 0.3999999999936145190, 0.5999999999936139750, 1.000000000000000000),
 ( 0.2500000000000000000, 0.2499999999968069986, 0.2999999999952105423, 0.3999999999936145190, 0.5999999999936139750, 1.000000000000000000),
 ( 0.2500000000000000000, 0.2499999999968069986, 0.2999999999952105423, 0.3999999999936145190, 0.5999999999936139750, 1.000000000000000000),
 ( 0.2500000000000000000, 0.2499999999968069986, 0.2999999999952105423, 0.3999999999936145190, 0.5999999999936139750, 1.000000000000000000),
 ( 0.2500000000000000000, 0.2499999999968069986, 0.2999999999952105423, 0.3999999999936145190, 0.5999999999936139750, 1.000000000000000000),
 ( 0.2500000000000000000, 0.2499999999968069986, 0.2999999999952105423, 0.3999999999936145190, 0.5999999999936139750, 1.000000000000000000),
 ( 0.2500000000000000000, 0.2499999999968069986, 0.2999999999952105423, 0.3999999999936145190, 0.5999999999936139750, 1.000000000000000000),
 ( 0.2500000000000000000, 0.2499999999968069986, 0.2999999999952105423, 0.3999999999936145190, 0.5999999999936139750, 1.000000000000000000) ) ) 
 REPRESENTATION_ITEM ( '' )  SURFACE ( )  );
#1175 = VECTOR ( 'NONE', #18133, 999.9999999999998863 ) ;
#1176 = DIRECTION ( 'NONE',  ( -0.000000000000000000, 1.000000000000000000, 0.000000000000000000 ) ) ;
#1177 = DIRECTION ( 'NONE',  ( 1.000000000000000000, 0.000000000000000000, -2.257453483404484831E-12 ) ) ;
#1178 = VERTEX_POINT ( 'NONE', #7211 ) ;
#1179 = CARTESIAN_POINT ( 'NONE',  ( -28.80902675589999973, 36.08666534569999840, -139.5659208849999970 ) ) ;
#1180 = EDGE_CURVE ( 'NONE', #7409, #9410, #21742, .T. ) ;
#1181 = FACE_OUTER_BOUND ( 'NONE', #20198, .T. ) ;
#1182 = CARTESIAN_POINT ( 'NONE',  ( 23.28094649261545612, 39.42349012523344243, -150.0552959530000123 ) ) ;
#1183 = ORIENTED_EDGE ( 'NONE', *, *, #4487, .T. ) ;
#1184 = DIRECTION ( 'NONE',  ( 1.000000000000000000, -5.094701932209999624E-24, -2.257144641399999941E-12 ) ) ;
#1185 = DIRECTION ( 'NONE',  ( 0.4472766253858966867, 0.8943956732807937238, -3.322738909413859124E-13 ) ) ;
#1186 = VERTEX_POINT ( 'NONE', #11465 ) ;
#1187 =( NAMED_UNIT ( * ) SI_UNIT ( $, .STERADIAN. ) SOLID_ANGLE_UNIT ( ) );
#1188 = DIRECTION ( 'NONE',  ( 1.000000000000000000, 0.000000000000000000, -2.257144641399999941E-12 ) ) ;
#1189 = AXIS2_PLACEMENT_3D ( 'NONE', #19887, #9150, #19642 ) ;
#1190 = PRESENTATION_LAYER_ASSIGNMENT (  '', '', ( #22450 ) ) ;
#1191 = ORIENTED_EDGE ( 'NONE', *, *, #8125, .F. ) ;
#1192 = FACE_OUTER_BOUND ( 'NONE', #10960, .T. ) ;
#1193 = LINE ( 'NONE', #15225, #13000 ) ;
#1194 = VERTEX_POINT ( 'NONE', #4102 ) ;
#1195 = DIRECTION ( 'NONE',  ( 1.000000000000000000, 2.004714280773594901E-17, -1.095180403012019938E-17 ) ) ;
#1196 = CARTESIAN_POINT ( 'NONE',  ( -25.59027027610704508, 34.17788759730120063, -140.1904131873745314 ) ) ;
#1197 = ORIENTED_EDGE ( 'NONE', *, *, #22760, .F. ) ;
#1198 =( LENGTH_UNIT ( ) NAMED_UNIT ( * ) SI_UNIT ( .MILLI., .METRE. ) );
#1199 = PRODUCT_DEFINITION_SHAPE ( 'NONE', 'NONE',  #3542 ) ;
#1200 = CARTESIAN_POINT ( 'NONE',  ( 2.068499633510000102, -14.99362786250000035, -147.5552959529999839 ) ) ;
#1201 = ORIENTED_EDGE ( 'NONE', *, *, #14324, .T. ) ;
#1202 = CARTESIAN_POINT ( 'NONE',  ( -21.35824191589999899, -4.000000000000000000, -144.8157682190000060 ) ) ;
#1203 = LINE ( 'NONE', #15346, #6548 ) ;
#1204 = ORIENTED_EDGE ( 'NONE', *, *, #16657, .F. ) ;
#1205 = LINE ( 'NONE', #2743, #20140 ) ;
#1206 = LINE ( 'NONE', #15458, #23527 ) ;
#1207 = CARTESIAN_POINT ( 'NONE',  ( -25.86630785139999844, -51.50000000000000000, -136.5552959530000123 ) ) ;
#1208 = VECTOR ( 'NONE', #21514, 1000.000000000000114 ) ;
#1209 = CIRCLE ( 'NONE', #14861, 2.500000000000000444 ) ;
#1210 = ADVANCED_FACE ( 'NONE', ( #656 ), #13255, .T. ) ;
#1211 = EDGE_CURVE ( 'NONE', #6134, #15113, #9565, .T. ) ;
#1212 = ORIENTED_EDGE ( 'NONE', *, *, #5354, .T. ) ;
#1213 = DIRECTION ( 'NONE',  ( -1.000000000000000000, -3.994014904670000134E-29, 2.423380700840000070E-27 ) ) ;
#1214 = CARTESIAN_POINT ( 'NONE',  ( -18.35824191589999899, -34.50000000000000000, -150.0657682190000060 ) ) ;
#1215 = CARTESIAN_POINT ( 'NONE',  ( -15.17828643429606039, 39.13746915041387808, -146.9793796816204008 ) ) ;
#1216 = DIRECTION ( 'NONE',  ( 1.000000000000000000, -5.094701932209999624E-24, 0.000000000000000000 ) ) ;
#1217 = VERTEX_POINT ( 'NONE', #20763 ) ;
#1218 = LINE ( 'NONE', #2868, #2873 ) ;
#1219 = CARTESIAN_POINT ( 'NONE',  ( 20.49999999999999645, -20.10730091830128430, -150.0552959529999839 ) ) ;
#1220 = CARTESIAN_POINT ( 'NONE',  ( -28.47499893025936046, 37.06529344306884610, -140.4421442387223635 ) ) ;
#1221 = CARTESIAN_POINT ( 'NONE',  ( 12.81474735470000148, -17.96536370379999781, -144.5552959529999839 ) ) ;
#1222 = CARTESIAN_POINT ( 'NONE',  ( -15.00000000000000000, -43.00000000000000000, -137.0552959530000123 ) ) ;
#1223 = VECTOR ( 'NONE', #7853, 1000.000000000000000 ) ;
#1224 = ORIENTED_EDGE ( 'NONE', *, *, #1675, .T. ) ;
#1225 = AXIS2_PLACEMENT_3D ( 'NONE', #4775, #17268, #977 ) ;
#1226 = DIRECTION ( 'NONE',  ( 0.000000000000000000, 2.256988247010000033E-12, 1.000000000000000000 ) ) ;
#1227 = DIRECTION ( 'NONE',  ( 1.734728570689999873E-18, 1.000000000000000000, 0.000000000000000000 ) ) ;
#1228 = CARTESIAN_POINT ( 'NONE',  ( -6.120427241202767377, -15.12266568073683537, -143.5552959530020019 ) ) ;
#1229 = DIRECTION ( 'NONE',  ( -1.000000000000000000, 0.000000000000000000, 0.000000000000000000 ) ) ;
#1230 = CARTESIAN_POINT ( 'NONE',  ( 3.611688725869999975E-11, -50.50000000000000000, -136.0552959530000123 ) ) ;
#1231 = EDGE_CURVE ( 'NONE', #9331, #22451, #7548, .T. ) ;
#1232 = ORIENTED_EDGE ( 'NONE', *, *, #20162, .F. ) ;
#1233 = CARTESIAN_POINT ( 'NONE',  ( -9.244908380075797183, 34.43529505381081890, -147.2272989846510427 ) ) ;
#1234 = CARTESIAN_POINT ( 'NONE',  ( 3.611688725869999975E-11, 20.96379895120000114, -136.0552959530000123 ) ) ;
#1235 = CARTESIAN_POINT ( 'NONE',  ( 3.190548969991207962, -2.742602116062627271, -150.0552959529999839 ) ) ;
#1236 = ORIENTED_EDGE ( 'NONE', *, *, #2105, .F. ) ;
#1237 = CARTESIAN_POINT ( 'NONE',  ( -29.52942110880598037, 36.03607219280863916, -139.7545453072953023 ) ) ;
#1238 = AXIS2_PLACEMENT_3D ( 'NONE', #1926, #9145, #135 ) ;
#1239 = EDGE_CURVE ( 'NONE', #16039, #2454, #13379, .T. ) ;
#1240 = CIRCLE ( 'NONE', #2374, 1.499999999999998446 ) ;
#1241 = DIRECTION ( 'NONE',  ( 0.000000000000000000, 0.000000000000000000, 1.000000000000000000 ) ) ;
#1242 = VERTEX_POINT ( 'NONE', #22082 ) ;
#1243 = AXIS2_PLACEMENT_3D ( 'NONE', #5508, #19671, #7170 ) ;
#1244 = CARTESIAN_POINT ( 'NONE',  ( -23.41273968116292892, 40.49448598672354649, -143.7690349874483218 ) ) ;
#1245 = DIRECTION ( 'NONE',  ( 5.094701932209999624E-24, 1.000000000000000000, -1.149947916579999802E-35 ) ) ;
#1246 = LINE ( 'NONE', #17642, #21560 ) ;
#1247 = DIRECTION ( 'NONE',  ( 1.000000000000000000, 0.000000000000000000, 0.000000000000000000 ) ) ;
#1248 = VERTEX_POINT ( 'NONE', #15169 ) ;
#1249 = CARTESIAN_POINT ( 'NONE',  ( -4.780317782130000914, 38.61135856239999953, -140.5115181619999873 ) ) ;
#1250 = CARTESIAN_POINT ( 'NONE',  ( 22.33963087269999903, -30.94765732060000119, -146.5552959529999839 ) ) ;
#1251 = CARTESIAN_POINT ( 'NONE',  ( -9.157754307290000284, -15.75963164970000108, -147.5552959529999839 ) ) ;
#1252 = EDGE_CURVE ( 'NONE', #14970, #1892, #16838, .T. ) ;
#1253 = ORIENTED_EDGE ( 'NONE', *, *, #20561, .T. ) ;
#1254 = ORIENTED_EDGE ( 'NONE', *, *, #6417, .F. ) ;
#1255 = CARTESIAN_POINT ( 'NONE',  ( -8.208807763381100742, 34.49436158464779822, -140.8229124830248224 ) ) ;
#1256 = CARTESIAN_POINT ( 'NONE',  ( 4.499999999879999102, -3.500000000000000000, -143.0552959529999839 ) ) ;
#1257 = DIRECTION ( 'NONE',  ( -2.602084747549999882E-17, 1.000000000000000000, 5.873624107189999522E-29 ) ) ;
#1258 = AXIS2_PLACEMENT_3D ( 'NONE', #6292, #9969, #17243 ) ;
#1259 = EDGE_CURVE ( 'NONE', #3932, #4709, #8360, .T. ) ;
#1260 = ORIENTED_EDGE ( 'NONE', *, *, #90, .T. ) ;
#1261 = DIRECTION ( 'NONE',  ( 0.7633862853691524286, 0.6459422414661292189, -7.105427357551423529E-15 ) ) ;
#1262 = DIRECTION ( 'NONE',  ( 0.000000000000000000, 0.000000000000000000, 1.000000000000000000 ) ) ;
#1263 = EDGE_CURVE ( 'NONE', #7782, #4750, #9320, .T. ) ;
#1264 = EDGE_LOOP ( 'NONE', ( #18506, #9337, #16865, #8986 ) ) ;
#1265 = DIRECTION ( 'NONE',  ( 2.257144641399999941E-12, 0.000000000000000000, 1.000000000000000000 ) ) ;
#1266 = EDGE_CURVE ( 'NONE', #18017, #12077, #18743, .T. ) ;
#1267 = EDGE_CURVE ( 'NONE', #22797, #7563, #11340, .T. ) ;
#1268 = CARTESIAN_POINT ( 'NONE',  ( -17.78691755432707566, 40.45100730230187480, -143.6151573293873298 ) ) ;
#1269 = CARTESIAN_POINT ( 'NONE',  ( -16.20076496858231963, -43.91979154561150267, -150.0552959529999839 ) ) ;
#1270 = CARTESIAN_POINT ( 'NONE',  ( 7.270619713791125704, -46.69911951120823090, -136.0552959530163832 ) ) ;
#1271 = CARTESIAN_POINT ( 'NONE',  ( -6.093288228365017822, 36.94882630176448401, -147.6373263597673713 ) ) ;
#1272 = CARTESIAN_POINT ( 'NONE',  ( -25.64408091310000160, 33.16124342930000068, -144.5387451670000019 ) ) ;
#1273 = CARTESIAN_POINT ( 'NONE',  ( 5.419791545609164984, -4.700764968563650115, -150.0552959529999555 ) ) ;
#1274 = PRESENTATION_LAYER_ASSIGNMENT (  '', '', ( #20269 ) ) ;
#1275 = CARTESIAN_POINT ( 'NONE',  ( -3.499999999969999998, 42.50000000000000000, -136.5552959530000123 ) ) ;
#1276 = VERTEX_POINT ( 'NONE', #14824 ) ;
#1277 = DIRECTION ( 'NONE',  ( -1.000000000000000000, 5.094701932209999624E-24, 0.000000000000000000 ) ) ;
#1278 = EDGE_CURVE ( 'NONE', #14591, #5107, #14936, .T. ) ;
#1279 = ORIENTED_EDGE ( 'NONE', *, *, #2845, .T. ) ;
#1280 = ORIENTED_EDGE ( 'NONE', *, *, #16797, .F. ) ;
#1281 = EDGE_LOOP ( 'NONE', ( #19318, #13543, #14266, #17955 ) ) ;
#1282 = CARTESIAN_POINT ( 'NONE',  ( 4.554119375355614174, 27.76008370043819795, -136.0552959530103294 ) ) ;
#1283 = CARTESIAN_POINT ( 'NONE',  ( 2.016283561950000358, -13.16498300129999954, -143.5552959529999839 ) ) ;
#1284 = ORIENTED_EDGE ( 'NONE', *, *, #17779, .T. ) ;
#1285 = EDGE_CURVE ( 'NONE', #18664, #7623, #16593, .T. ) ;
#1286 = VERTEX_POINT ( 'NONE', #18625 ) ;
#1287 = DIRECTION ( 'NONE',  ( 0.000000000000000000, 0.000000000000000000, -1.000000000000000000 ) ) ;
#1288 = CARTESIAN_POINT ( 'NONE',  ( -9.483015687270000882, 40.53201449259999833, -146.0034198470000035 ) ) ;
#1289 = EDGE_CURVE ( 'NONE', #17090, #1341, #2215, .T. ) ;
#1290 = CARTESIAN_POINT ( 'NONE',  ( -11.40498010996960332, 39.09966106399821228, -141.2721109090012419 ) ) ;
#1291 = AXIS2_PLACEMENT_3D ( 'NONE', #14503, #21767, #18645 ) ;
#1292 = CARTESIAN_POINT ( 'NONE',  ( -21.74973190997081929, -3.330829822294064435, -146.3157682189990680 ) ) ;
#1293 = CARTESIAN_POINT ( 'NONE',  ( -7.427142538590000065, 36.18616221519999954, -139.9783837409999876 ) ) ;
#1294 = CARTESIAN_POINT ( 'NONE',  ( -9.241517523749537943, 39.86784999477015390, -147.9446264559352926 ) ) ;
#1295 = ORIENTED_EDGE ( 'NONE', *, *, #21347, .T. ) ;
#1296 = CARTESIAN_POINT ( 'NONE',  ( -28.14969746239999893, 32.41805236249999922, -143.4814202869999917 ) ) ;
#1297 = CARTESIAN_POINT ( 'NONE',  ( 5.810679582541388832, -4.255428470556350540, -136.0552959530029682 ) ) ;
#1298 = DIRECTION ( 'NONE',  ( -2.250785033110000127E-12, 0.000000000000000000, -1.000000000000000000 ) ) ;
#1299 = ORIENTED_EDGE ( 'NONE', *, *, #1110, .F. ) ;
#1300 = DIRECTION ( 'NONE',  ( 0.7071067811865473507, 0.7071067811865477948, 0.000000000000000000 ) ) ;
#1301 = VERTEX_POINT ( 'NONE', #20648 ) ;
#1302 = LINE ( 'NONE', #21401, #6387 ) ;
#1303 = CARTESIAN_POINT ( 'NONE',  ( -7.337311498540000088, -24.10744501490000147, -147.5552959529999839 ) ) ;
#1304 = ORIENTED_EDGE ( 'NONE', *, *, #5149, .F. ) ;
#1305 = CARTESIAN_POINT ( 'NONE',  ( 8.302653104916485560, 38.49041384248582176, -146.0625927866742870 ) ) ;
#1306 = DIRECTION ( 'NONE',  ( 1.000000000000000000, -5.094701932209999624E-24, 0.000000000000000000 ) ) ;
#1307 = ORIENTED_EDGE ( 'NONE', *, *, #10406, .T. ) ;
#1308 = VECTOR ( 'NONE', #949, 1000.000000000000000 ) ;
#1309 = CARTESIAN_POINT ( 'NONE',  ( -9.812199629320000227, -24.40642616239999896, -147.5552959529999839 ) ) ;
#1310 = CARTESIAN_POINT ( 'NONE',  ( -25.30868096333427175, 35.35627366547125661, -147.9647939034089461 ) ) ;
#1311 = ORIENTED_EDGE ( 'NONE', *, *, #15794, .F. ) ;
#1312 =( BOUNDED_SURFACE ( )  B_SPLINE_SURFACE ( 5, 5, ( 
 ( #12886, #22177, #2194, #2543, #11555, #18728 ),
 ( #16816, #2437, #9546, #22289, #528, #17042 ),
 ( #18602, #5978, #3972, #20511, #9765, #7761 ),
 ( #15026, #9654, #18833, #16929, #638, #20167 ),
 ( #4325, #7647, #9417, #7871, #3860, #2083 ),
 ( #20279, #4083, #16694, #15146, #5861, #18372 ),
 ( #22409, #6105, #20391, #7991, #409, #13360 ),
 ( #9301, #11095, #11321, #20630, #14918, #761 ),
 ( #15275, #16577, #285, #7527, #13120, #14802 ),
 ( #22063, #5751, #13009, #11205, #18479, #10125 ),
 ( #4556, #15845, #17399, #1118, #11918, #22888 ),
 ( #997, #3133, #11794, #19073, #17639, #1348 ) ),
 .UNSPECIFIED., .F., .F., .F. ) 
 B_SPLINE_SURFACE_WITH_KNOTS ( ( 6, 3, 3, 6 ),
 ( 6, 6 ),
 ( 0.000000000000000000, 4.066159495680000013, 8.252146144990000209, 12.56898909050000057 ),
 ( 0.000000000000000000, 1.570796326821630062 ),
 .UNSPECIFIED. ) 
 GEOMETRIC_REPRESENTATION_ITEM ( )  RATIONAL_B_SPLINE_SURFACE ( (
 ( 1.000000000000000000, 0.5999999999932189576, 0.3999999999932190020, 0.2999999999949140017, 0.2499999999966094899, 0.2500000000000000000),
 ( 1.000000000000000000, 0.5999999999932189576, 0.3999999999932190020, 0.2999999999949140017, 0.2499999999966094899, 0.2500000000000000000),
 ( 1.000000000000000000, 0.5999999999932189576, 0.3999999999932190020, 0.2999999999949140017, 0.2499999999966094899, 0.2500000000000000000),
 ( 1.000000000000000000, 0.5999999999932189576, 0.3999999999932190020, 0.2999999999949140017, 0.2499999999966094899, 0.2500000000000000000),
 ( 1.000000000000000000, 0.5999999999932189576, 0.3999999999932190020, 0.2999999999949140017, 0.2499999999966094899, 0.2500000000000000000),
 ( 1.000000000000000000, 0.5999999999932189576, 0.3999999999932190020, 0.2999999999949140017, 0.2499999999966094899, 0.2500000000000000000),
 ( 1.000000000000000000, 0.5999999999932189576, 0.3999999999932190020, 0.2999999999949140017, 0.2499999999966094899, 0.2500000000000000000),
 ( 1.000000000000000000, 0.5999999999932189576, 0.3999999999932190020, 0.2999999999949140017, 0.2499999999966094899, 0.2500000000000000000),
 ( 1.000000000000000000, 0.5999999999932189576, 0.3999999999932190020, 0.2999999999949140017, 0.2499999999966094899, 0.2500000000000000000),
 ( 1.000000000000000000, 0.5999999999932189576, 0.3999999999932190020, 0.2999999999949140017, 0.2499999999966094899, 0.2500000000000000000),
 ( 1.000000000000000000, 0.5999999999932189576, 0.3999999999932190020, 0.2999999999949140017, 0.2499999999966094899, 0.2500000000000000000),
 ( 1.000000000000000000, 0.5999999999932189576, 0.3999999999932190020, 0.2999999999949140017, 0.2499999999966094899, 0.2500000000000000000) ) ) 
 REPRESENTATION_ITEM ( '' )  SURFACE ( )  );
#1313 = EDGE_CURVE ( 'NONE', #18451, #1301, #8009, .T. ) ;
#1314 = ORIENTED_EDGE ( 'NONE', *, *, #19463, .T. ) ;
#1315 = CARTESIAN_POINT ( 'NONE',  ( 32.50000000000000000, 20.96379895120000114, -137.0552959530000123 ) ) ;
#1316 = CARTESIAN_POINT ( 'NONE',  ( -32.50000000000000000, 47.50000000000000000, -151.0552959529999839 ) ) ;
#1317 = ORIENTED_EDGE ( 'NONE', *, *, #12829, .F. ) ;
#1318 = DIRECTION ( 'NONE',  ( 1.000000000000000000, 0.000000000000000000, 0.000000000000000000 ) ) ;
#1319 = B_SPLINE_CURVE_WITH_KNOTS ( 'NONE', 5,
 ( #12966, #8913, #20244, #3936, #8801, #16196, #16078, #23448, #7144, #14409, #11403, #22487 ),
 .UNSPECIFIED., .F., .F.,
 ( 6, 3, 3, 6 ),
 ( 0.000000000000000000, 4.066159495680000013, 8.252146144990000209, 12.56898909049999880 ),
 .UNSPECIFIED. ) ;
#1320 = CARTESIAN_POINT ( 'NONE',  ( 31.50000000000000000, -0.1159497378070000057, -149.5552959529999839 ) ) ;
#1321 = CARTESIAN_POINT ( 'NONE',  ( -1.550733472753473619, 45.02071668630011203, -136.0552959529965165 ) ) ;
#1322 = ORIENTED_EDGE ( 'NONE', *, *, #3520, .T. ) ;
#1323 = CARTESIAN_POINT ( 'NONE',  ( -6.683153925719999222, -51.50000000000000000, -150.0552959529999839 ) ) ;
#1324 = FACE_OUTER_BOUND ( 'NONE', #21450, .T. ) ;
#1325 = CARTESIAN_POINT ( 'NONE',  ( -14.01363760658083457, 39.11235265668859995, -141.1958727404175136 ) ) ;
#1326 = FACE_OUTER_BOUND ( 'NONE', #18212, .T. ) ;
#1327 = EDGE_LOOP ( 'NONE', ( #7904, #19498, #22770, #2319 ) ) ;
#1328 = PLANE ( 'NONE',  #6291 ) ;
#1329 = FACE_OUTER_BOUND ( 'NONE', #21772, .T. ) ;
#1330 = CARTESIAN_POINT ( 'NONE',  ( 19.68320006079999729, -16.50000000000000000, -150.0552959529999839 ) ) ;
#1331 = CARTESIAN_POINT ( 'NONE',  ( -10.88504013565279216, 37.01634837951832679, -139.4704149078483226 ) ) ;
#1332 = DIRECTION ( 'NONE',  ( 2.257157423930000049E-12, 0.000000000000000000, 1.000000000000000000 ) ) ;
#1333 = ORIENTED_EDGE ( 'NONE', *, *, #4730, .T. ) ;
#1334 = CARTESIAN_POINT ( 'NONE',  ( -16.17668464575115195, 34.89952366001249828, -140.8770501902727119 ) ) ;
#1335 = EDGE_CURVE ( 'NONE', #322, #21462, #16714, .T. ) ;
#1336 = CARTESIAN_POINT ( 'NONE',  ( -26.47299999999999898, 14.00000000000000000, -144.0552959529999839 ) ) ;
#1337 = CARTESIAN_POINT ( 'NONE',  ( 1.000000000140000012, 41.50000000000000000, -147.0552959529999839 ) ) ;
#1338 = DIRECTION ( 'NONE',  ( 2.839308199620000013E-14, 3.568879590630000244E-13, 1.000000000000000000 ) ) ;
#1339 = ADVANCED_FACE ( 'NONE', ( #9672 ), #18852, .T. ) ;
#1340 = DIRECTION ( 'NONE',  ( 0.000000000000000000, -1.000000000000000000, 0.000000000000000000 ) ) ;
#1341 = VERTEX_POINT ( 'NONE', #7667 ) ;
#1342 = DIRECTION ( 'NONE',  ( 1.000000000000000000, 0.000000000000000000, -2.257453483404482811E-12 ) ) ;
#1343 = CARTESIAN_POINT ( 'NONE',  ( -25.17490547269999723, 35.46855981759999565, -147.6699473629999773 ) ) ;
#1344 = ORIENTED_EDGE ( 'NONE', *, *, #21880, .F. ) ;
#1345 = CARTESIAN_POINT ( 'NONE',  ( -29.68301555210662102, 36.92109708053965988, -140.1550845752753105 ) ) ;
#1346 = PLANE ( 'NONE',  #12894 ) ;
#1347 = VERTEX_POINT ( 'NONE', #15293 ) ;
#1348 = CARTESIAN_POINT ( 'NONE',  ( -14.11967125442052051, 36.98834135278355717, -140.5455248811183822 ) ) ;
#1349 = CARTESIAN_POINT ( 'NONE',  ( 6.500000000140000012, 20.50000000000000000, -147.5552959529999839 ) ) ;
#1350 = LINE ( 'NONE', #10594, #19286 ) ;
#1351 = CARTESIAN_POINT ( 'NONE',  ( 7.073008394724321413, 36.53702466590743114, -141.5985056069079633 ) ) ;
#1352 = AXIS2_PLACEMENT_3D ( 'NONE', #1566, #5353, #12601 ) ;
#1353 = ORIENTED_EDGE ( 'NONE', *, *, #15122, .T. ) ;
#1354 = CARTESIAN_POINT ( 'NONE',  ( -5.251527070960000820, 40.93408815870000694, -143.6492421949999994 ) ) ;
#1355 = DIRECTION ( 'NONE',  ( 0.000000000000000000, 0.000000000000000000, 1.000000000000000000 ) ) ;
#1356 = CARTESIAN_POINT ( 'NONE',  ( -8.564938780319947043, 40.19157471905271706, -145.9271927685878154 ) ) ;
#1357 = DIRECTION ( 'NONE',  ( 0.000000000000000000, 0.000000000000000000, 1.000000000000000000 ) ) ;
#1358 = ORIENTED_EDGE ( 'NONE', *, *, #1231, .T. ) ;
#1359 = VERTEX_POINT ( 'NONE', #3990 ) ;
#1360 = CARTESIAN_POINT ( 'NONE',  ( -7.902404225063866861, 35.56594207916549522, -140.9322834864426852 ) ) ;
#1361 = CARTESIAN_POINT ( 'NONE',  ( -5.459597139290000456, 36.94776568910000236, -139.8191173760000083 ) ) ;
#1362 = ADVANCED_FACE ( 'NONE', ( #11224 ), #18497, .T. ) ;
#1363 = DIRECTION ( 'NONE',  ( 1.457985068979999943E-12, 1.723073263340000007E-12, -1.000000000000000000 ) ) ;
#1364 = VERTEX_POINT ( 'NONE', #21003 ) ;
#1365 = DIRECTION ( 'NONE',  ( 1.000000000000000000, 3.994014904670000134E-29, -2.423380700840000070E-27 ) ) ;
#1366 = CARTESIAN_POINT ( 'NONE',  ( 2.500000000150000012, 24.50000000000000000, -143.5552959529999839 ) ) ;
#1367 = VECTOR ( 'NONE', #19078, 1000.000000000000000 ) ;
#1368 = VECTOR ( 'NONE', #16491, 1000.000000000000000 ) ;
#1369 = VERTEX_POINT ( 'NONE', #15757 ) ;
#1370 = CARTESIAN_POINT ( 'NONE',  ( -32.50000000000000000, 19.50000000000000000, -151.0552959529999839 ) ) ;
#1371 = EDGE_CURVE ( 'NONE', #21536, #6962, #23017, .T. ) ;
#1372 = CARTESIAN_POINT ( 'NONE',  ( -18.90246017567791270, 37.04541408822704796, -147.4848489022495528 ) ) ;
#1373 = CARTESIAN_POINT ( 'NONE',  ( -20.60824191591068555, -4.000000000000000000, -141.9623572383543717 ) ) ;
#1374 = CARTESIAN_POINT ( 'NONE',  ( 4.750000000030004443, -45.01539404905023645, -136.0552959530107273 ) ) ;
#1375 = DIRECTION ( 'NONE',  ( 0.000000000000000000, 0.000000000000000000, -1.000000000000000000 ) ) ;
#1376 = CARTESIAN_POINT ( 'NONE',  ( -16.92867099909999595, 34.38083942290000294, -140.2753207150000208 ) ) ;
#1377 = CARTESIAN_POINT ( 'NONE',  ( -3.499999999920000437, 40.00000000000000000, -135.0552959530000123 ) ) ;
#1378 = DIRECTION ( 'NONE',  ( -0.9840552701943220404, 0.1778629393740580045, -3.651917849741195385E-14 ) ) ;
#1379 = EDGE_CURVE ( 'NONE', #9692, #10188, #2914, .T. ) ;
#1380 = VERTEX_POINT ( 'NONE', #20883 ) ;
#1381 = VECTOR ( 'NONE', #3456, 1000.000000000000000 ) ;
#1382 = CARTESIAN_POINT ( 'NONE',  ( -22.52780672251092042, 37.05898997718767873, -140.0074087193914067 ) ) ;
#1383 = VECTOR ( 'NONE', #7873, 1000.000000000000114 ) ;
#1384 = UNCERTAINTY_MEASURE_WITH_UNIT (LENGTH_MEASURE( 1.000000000000000082E-05 ), #11513, 'distance_accuracy_value', 'NONE');
#1385 = ADVANCED_FACE ( 'NONE', ( #15865 ), #13608, .F. ) ;
#1386 = VERTEX_POINT ( 'NONE', #8243 ) ;
#1387 = VERTEX_POINT ( 'NONE', #19325 ) ;
#1388 = LINE ( 'NONE', #17678, #17059 ) ;
#1389 = LINE ( 'NONE', #3062, #2353 ) ;
#1390 = EDGE_LOOP ( 'NONE', ( #8124, #20683, #10522, #22148 ) ) ;
#1391 = ORIENTED_EDGE ( 'NONE', *, *, #18377, .F. ) ;
#1392 = DIRECTION ( 'NONE',  ( 0.000000000000000000, 1.000000000000000000, 0.000000000000000000 ) ) ;
#1393 = DIRECTION ( 'NONE',  ( 1.000000000000000000, 0.000000000000000000, 0.000000000000000000 ) ) ;
#1394 = CARTESIAN_POINT ( 'NONE',  ( -12.13467478890487961, 40.69160539512103725, -144.5327625259997717 ) ) ;
#1395 = PLANE ( 'NONE',  #13593 ) ;
#1396 = CARTESIAN_POINT ( 'NONE',  ( -8.249050749313617814, 34.24288854963995732, -140.4966857150371595 ) ) ;
#1397 = ORIENTED_EDGE ( 'NONE', *, *, #13616, .T. ) ;
#1398 = EDGE_CURVE ( 'NONE', #23370, #2980, #10145, .T. ) ;
#1399 = CARTESIAN_POINT ( 'NONE',  ( 9.693958997696052293, 36.09174344073587548, -141.7260982849746540 ) ) ;
#1400 = VECTOR ( 'NONE', #9278, 1000.000000000000000 ) ;
#1401 = EDGE_CURVE ( 'NONE', #21066, #12006, #19779, .T. ) ;
#1402 = CARTESIAN_POINT ( 'NONE',  ( -21.35824191589999899, -32.75000000000000000, -144.8157682190000060 ) ) ;
#1403 = DIRECTION ( 'NONE',  ( -1.000000000000000000, 0.000000000000000000, 2.257076750620000196E-12 ) ) ;
#1404 = B_SPLINE_CURVE_WITH_KNOTS ( 'NONE', 1,
 ( #18749, #9917 ),
 .UNSPECIFIED., .F., .F.,
 ( 2, 2 ),
 ( -6.000000000000000000, 6.000000000000000000 ),
 .UNSPECIFIED. ) ;
#1405 = EDGE_LOOP ( 'NONE', ( #12527, #20995, #14025, #12342, #16570, #13119 ) ) ;
#1406 = EDGE_CURVE ( 'NONE', #3396, #4045, #8593, .T. ) ;
#1407 = ADVANCED_FACE ( 'NONE', ( #12178 ), #12055, .F. ) ;
#1408 = DIRECTION ( 'NONE',  ( 0.000000000000000000, -1.000000000000000000, 3.568879590630000244E-13 ) ) ;
#1409 = ORIENTED_EDGE ( 'NONE', *, *, #7932, .F. ) ;
#1410 = CARTESIAN_POINT ( 'NONE',  ( -19.69393976310000127, 37.84845892290000080, -140.3168504270000199 ) ) ;
#1411 = FACE_OUTER_BOUND ( 'NONE', #3594, .T. ) ;
#1412 = EDGE_CURVE ( 'NONE', #2388, #15779, #6827, .T. ) ;
#1414 = ORIENTED_EDGE ( 'NONE', *, *, #13034, .F. ) ;
#1413 = AXIS2_PLACEMENT_3D ( 'NONE', #13472, #17045, #4794 ) ;
#1415 = CARTESIAN_POINT ( 'NONE',  ( -20.45144833149999997, 36.94873838139999833, -139.8044047869999815 ) ) ;
#1416 = CARTESIAN_POINT ( 'NONE',  ( -6.366307851350000213, 50.50000000000000000, -136.0552959530000123 ) ) ;
#1417 = EDGE_LOOP ( 'NONE', ( #11256, #21139, #23417, #7533 ) ) ;
#1418 = CARTESIAN_POINT ( 'NONE',  ( -15.96393590121257233, 38.83090064245826056, -147.9761310711117801 ) ) ;
#1419 = EDGE_CURVE ( 'NONE', #22886, #9252, #5700, .T. ) ;
#1420 = AXIS2_PLACEMENT_3D ( 'NONE', #23084, #17844, #15817 ) ;
#1421 = CARTESIAN_POINT ( 'NONE',  ( -27.77832206610000298, 37.03059619289999915, -147.6270870419999710 ) ) ;
#1422 = VERTEX_POINT ( 'NONE', #4812 ) ;
#1423 = CARTESIAN_POINT ( 'NONE',  ( 0.000000000000000000, 0.000000000000000000, 0.000000000000000000 ) ) ;
#1424 = VERTEX_POINT ( 'NONE', #21360 ) ;
#1425 = DIRECTION ( 'NONE',  ( 0.09606172499277226828, 0.9953753789357124848, -8.277822871607614780E-13 ) ) ;
#1426 = CARTESIAN_POINT ( 'NONE',  ( 14.79224200840030257, -34.50000000000000000, -149.4708568728852356 ) ) ;
#1427 = VERTEX_POINT ( 'NONE', #8372 ) ;
#1428 = LINE ( 'NONE', #7357, #3054 ) ;
#1429 = LINE ( 'NONE', #17483, #12868 ) ;
#1430 = ORIENTED_EDGE ( 'NONE', *, *, #14481, .F. ) ;
#1431 = CARTESIAN_POINT ( 'NONE',  ( -25.54709891120000265, 36.13246793440000459, -139.7173810940000180 ) ) ;
#1432 = VECTOR ( 'NONE', #22263, 1000.000000000000000 ) ;
#1433 = COLOUR_RGB ( '', 0.31764706, 0.68627451, 0.89019608) ;
#1434 = ORIENTED_EDGE ( 'NONE', *, *, #9513, .T. ) ;
#1435 = CARTESIAN_POINT ( 'NONE',  ( -5.499999999969999109, 44.50000000000000000, -137.0552959530000123 ) ) ;
#1436 = AXIS2_PLACEMENT_3D ( 'NONE', #3180, #6733, #14352 ) ;
#1437 = CARTESIAN_POINT ( 'NONE',  ( 1.133692148650000009, -51.50000000000000000, -136.0552959530000123 ) ) ;
#1438 = APPLICATION_CONTEXT ( 'automotive_design' ) ;
#1439 = EDGE_CURVE ( 'NONE', #1936, #23105, #902, .T. ) ;
#1440 = CARTESIAN_POINT ( 'NONE',  ( -15.03885004549999849, 41.12207116019999376, -146.4108951270000034 ) ) ;
#1441 = CARTESIAN_POINT ( 'NONE',  ( -28.71215957428060506, 38.99550079887305287, -140.7731748223484090 ) ) ;
#1442 = ORIENTED_EDGE ( 'NONE', *, *, #10525, .T. ) ;
#1443 = CARTESIAN_POINT ( 'NONE',  ( 23.50000000000000000, -20.50000000000000000, -137.0552959530000123 ) ) ;
#1444 = CARTESIAN_POINT ( 'NONE',  ( -13.50000000000000000, -43.00000000000000000, -150.0552959529999839 ) ) ;
#1445 = DIRECTION ( 'NONE',  ( 1.000000000000000000, 0.000000000000000000, 2.508689552389999873E-12 ) ) ;
#1446 = CARTESIAN_POINT ( 'NONE',  ( 18.95053822279999878, 51.50000000000000000, -149.5552959529999839 ) ) ;
#1447 = DIRECTION ( 'NONE',  ( 1.000000000000000000, 0.000000000000000000, 0.000000000000000000 ) ) ;
#1448 = ORIENTED_EDGE ( 'NONE', *, *, #5211, .F. ) ;
#1449 = LINE ( 'NONE', #5365, #8779 ) ;
#1450 = CIRCLE ( 'NONE', #6356, 2.500000000000000444 ) ;
#1451 = CARTESIAN_POINT ( 'NONE',  ( -13.79886907581265909, -42.07977154562041733, -136.0552959529688621 ) ) ;
#1452 = CARTESIAN_POINT ( 'NONE',  ( -6.366307851710000243, -51.50000000000000000, -136.0552959530000123 ) ) ;
#1453 = CIRCLE ( 'NONE', #17009, 2.000000000000000000 ) ;
#1454 = CARTESIAN_POINT ( 'NONE',  ( -34.97299999999999898, 11.80604359530000025, -145.2538597989999971 ) ) ;
#1455 = CARTESIAN_POINT ( 'NONE',  ( -31.50000000000000000, 19.50000000000000000, -149.5552959529999839 ) ) ;
#1456 = DIRECTION ( 'NONE',  ( 2.261079091466875261E-12, 0.000000000000000000, 1.000000000000000000 ) ) ;
#1457 = ORIENTED_EDGE ( 'NONE', *, *, #22542, .T. ) ;
#1458 = CARTESIAN_POINT ( 'NONE',  ( -6.165211177139999776, -15.11551140080000089, -142.5552959529999839 ) ) ;
#1459 = CARTESIAN_POINT ( 'NONE',  ( -2.499999999920000437, 40.00000000000000000, -135.0552959530000123 ) ) ;
#1460 = ORIENTED_EDGE ( 'NONE', *, *, #13738, .F. ) ;
#1461 = DIRECTION ( 'NONE',  ( 0.000000000000000000, -2.256894259950000208E-12, 1.000000000000000000 ) ) ;
#1462 = EDGE_CURVE ( 'NONE', #21680, #8156, #18971, .T. ) ;
#1463 = DIRECTION ( 'NONE',  ( 0.000000000000000000, -1.000000000000000000, 2.257453483404482811E-12 ) ) ;
#1464 = EDGE_LOOP ( 'NONE', ( #4342, #10992, #21636 ) ) ;
#1465 = CARTESIAN_POINT ( 'NONE',  ( 22.00000000000000000, -20.50000000000000000, -135.0552959530000123 ) ) ;
#1466 = AXIS2_PLACEMENT_3D ( 'NONE', #2201, #1978, #9551 ) ;
#1467 = ADVANCED_FACE ( 'NONE', ( #15641 ), #8127, .F. ) ;
#1468 = LINE ( 'NONE', #22996, #9330 ) ;
#1469 = AXIS2_PLACEMENT_3D ( 'NONE', #16156, #5197, #23295 ) ;
#1470 = LINE ( 'NONE', #7039, #16255 ) ;
#1471 = CARTESIAN_POINT ( 'NONE',  ( 7.209217092486989387, 36.23514394621652457, -141.6749984785230936 ) ) ;
#1472 = ORIENTED_EDGE ( 'NONE', *, *, #18009, .T. ) ;
#1473 = CARTESIAN_POINT ( 'NONE',  ( -11.46682130719020876, 35.35929522821826509, -140.3232393995872087 ) ) ;
#1474 = EDGE_CURVE ( 'NONE', #12438, #20510, #5173, .T. ) ;
#1475 = CARTESIAN_POINT ( 'NONE',  ( -18.60901166350398483, 37.01038625230250290, -148.6497975989814506 ) ) ;
#1476 = CARTESIAN_POINT ( 'NONE',  ( -8.764836022000000781, 39.53398178709999655, -147.5842891229999907 ) ) ;
#1477 = CARTESIAN_POINT ( 'NONE',  ( 5.298801200344347428, -31.10703351611365974, -136.0552959530119779 ) ) ;
#1478 = EDGE_LOOP ( 'NONE', ( #5603, #15343, #800, #15418 ) ) ;
#1479 = FACE_OUTER_BOUND ( 'NONE', #12093, .T. ) ;
#1480 = ORIENTED_EDGE ( 'NONE', *, *, #5903, .T. ) ;
#1481 = CARTESIAN_POINT ( 'NONE',  ( -6.901241125868466497, 36.34453081637710881, -147.4362978685941528 ) ) ;
#1482 = CARTESIAN_POINT ( 'NONE',  ( 32.50000000000000000, -33.03620104880000241, -136.5552959530000123 ) ) ;
#1483 = DIRECTION ( 'NONE',  ( -1.000000000000000000, 0.000000000000000000, 2.262079412673754432E-12 ) ) ;
#1484 = EDGE_CURVE ( 'NONE', #21680, #6936, #13736, .T. ) ;
#1485 = AXIS2_PLACEMENT_3D ( 'NONE', #19777, #12621, #18343 ) ;
#1486 = VERTEX_POINT ( 'NONE', #19677 ) ;
#1487 = CARTESIAN_POINT ( 'NONE',  ( -5.480550747686820046, 36.94526453639213059, -140.5641745855346301 ) ) ;
#1488 = CARTESIAN_POINT ( 'NONE',  ( -31.00000000000000000, 0.000000000000000000, -150.0552959529999839 ) ) ;
#1489 = AXIS2_PLACEMENT_3D ( 'NONE', #19639, #18090, #1802 ) ;
#1490 = EDGE_CURVE ( 'NONE', #4619, #22505, #18016, .T. ) ;
#1491 = ORIENTED_EDGE ( 'NONE', *, *, #21184, .T. ) ;
#1492 = FACE_OUTER_BOUND ( 'NONE', #7110, .T. ) ;
#1493 = CIRCLE ( 'NONE', #5705, 0.7500000000000006661 ) ;
#1494 = CIRCLE ( 'NONE', #4516, 0.7500000000000006661 ) ;
#1495 = LINE ( 'NONE', #12529, #7921 ) ;
#1496 = CARTESIAN_POINT ( 'NONE',  ( -15.39269908169872814, -40.00000000000000000, -150.0552959529999555 ) ) ;
#1497 = DIRECTION ( 'NONE',  ( 1.526468026909999897E-13, 8.159623473500000156E-13, 1.000000000000000000 ) ) ;
#1498 = EDGE_CURVE ( 'NONE', #11714, #23177, #21472, .T. ) ;
#1499 = CARTESIAN_POINT ( 'NONE',  ( 19.75551406279999966, -31.14090339520000228, -145.0552959529999839 ) ) ;
#1500 = DIRECTION ( 'NONE',  ( 2.256861364460000137E-12, 0.000000000000000000, 1.000000000000000000 ) ) ;
#1501 = PRODUCT_CONTEXT ( 'NONE', #3407, 'mechanical' ) ;
#1502 = DIRECTION ( 'NONE',  ( 0.000000000000000000, 1.000000000000000000, 0.000000000000000000 ) ) ;
#1503 = EDGE_CURVE ( 'NONE', #8311, #21143, #14320, .T. ) ;
#1504 = CARTESIAN_POINT ( 'NONE',  ( 6.500000000030000002, 20.50000000000000000, -137.0552959530000123 ) ) ;
#1505 = AXIS2_PLACEMENT_3D ( 'NONE', #2481, #16980, #20221 ) ;
#1506 = VECTOR ( 'NONE', #4741, 1000.000000000000000 ) ;
#1507 = VERTEX_POINT ( 'NONE', #1728 ) ;
#1508 = CARTESIAN_POINT ( 'NONE',  ( -23.43027330800707730, 37.94004033882730198, -139.4495095434923826 ) ) ;
#1509 = AXIS2_PLACEMENT_3D ( 'NONE', #1202, #9968, #19028 ) ;
#1510 = ORIENTED_EDGE ( 'NONE', *, *, #3866, .T. ) ;
#1511 = SURFACE_STYLE_FILL_AREA ( #12196 ) ;
#1512 = VECTOR ( 'NONE', #929, 1000.000000000000114 ) ;
#1513 = VERTEX_POINT ( 'NONE', #12648 ) ;
#1514 = CARTESIAN_POINT ( 'NONE',  ( -15.57786843150000067, 37.00666880280000726, -148.5521201120000114 ) ) ;
#1515 = CARTESIAN_POINT ( 'NONE',  ( -9.282104535849999394, -16.71402168319999859, -144.5552959529999839 ) ) ;
#1516 = LINE ( 'NONE', #8738, #9157 ) ;
#1517 = ORIENTED_EDGE ( 'NONE', *, *, #20608, .F. ) ;
#1518 = CARTESIAN_POINT ( 'NONE',  ( -5.660514123339918768, 20.09808825513541208, -150.0552959529999839 ) ) ;
#1519 = CARTESIAN_POINT ( 'NONE',  ( -9.771488485180000794, 38.65068379619999916, -147.6127673909999771 ) ) ;
#1520 = CARTESIAN_POINT ( 'NONE',  ( -11.27392315527871602, 41.29449409377051694, -144.7140135096667848 ) ) ;
#1521 = LINE ( 'NONE', #3403, #3341 ) ;
#1522 = VERTEX_POINT ( 'NONE', #1615 ) ;
#1523 = DIRECTION ( 'NONE',  ( -0.7633862853691524286, 0.6459422414661292189, -2.886579864030575227E-15 ) ) ;
#1524 = AXIS2_PLACEMENT_3D ( 'NONE', #17663, #8596, #15869 ) ;
#1525 = EDGE_CURVE ( 'NONE', #11936, #12077, #12293, .T. ) ;
#1526 = EDGE_LOOP ( 'NONE', ( #20689, #14688, #9788, #17546 ) ) ;
#1527 = VECTOR ( 'NONE', #2984, 1000.000000000000000 ) ;
#1528 = CARTESIAN_POINT ( 'NONE',  ( 9.488686602576935414, 35.87182884379176784, -141.8241438738831732 ) ) ;
#1529 = CONICAL_SURFACE ( 'NONE', #3036, 2.000000000000003553, 0.7853981633970000820 ) ;
#1530 = DIRECTION ( 'NONE',  ( 2.257144641397284947E-12, -2.714760815920564689E-24, 1.000000000000000000 ) ) ;
#1531 = AXIS2_PLACEMENT_3D ( 'NONE', #18208, #9370, #16534 ) ;
#1532 = DIRECTION ( 'NONE',  ( 1.000000000000000000, 0.000000000000000000, -2.775557561562891351E-14 ) ) ;
#1533 = EDGE_CURVE ( 'NONE', #17988, #2949, #23369, .T. ) ;
#1534 = ORIENTED_EDGE ( 'NONE', *, *, #9605, .F. ) ;
#1535 = FACE_OUTER_BOUND ( 'NONE', #6075, .T. ) ;
#1536 = EDGE_LOOP ( 'NONE', ( #20552, #1056, #13949, #18491 ) ) ;
#1537 = FACE_OUTER_BOUND ( 'NONE', #17839, .T. ) ;
#1538 = CARTESIAN_POINT ( 'NONE',  ( -30.49999999990000177, 26.50000000000000000, -140.5552959529999839 ) ) ;
#1539 = ORIENTED_EDGE ( 'NONE', *, *, #18978, .T. ) ;
#1540 = CARTESIAN_POINT ( 'NONE',  ( 26.50000000000000000, -20.50000000000000000, -150.0552959529999839 ) ) ;
#1541 = ORIENTED_EDGE ( 'NONE', *, *, #3184, .T. ) ;
#1542 = CARTESIAN_POINT ( 'NONE',  ( -21.54058924440989742, 34.11652205135742832, -147.8735334098300029 ) ) ;
#1543 = EDGE_CURVE ( 'NONE', #11590, #6997, #9059, .T. ) ;
#1544 = DIRECTION ( 'NONE',  ( 4.430318231639999944E-12, -6.100259101500000139E-13, 1.000000000000000000 ) ) ;
#1545 = EDGE_LOOP ( 'NONE', ( #12281, #19267, #14801, #9609 ) ) ;
#1546 = DIRECTION ( 'NONE',  ( 1.000000000000000000, 0.000000000000000000, 0.000000000000000000 ) ) ;
#1547 = VECTOR ( 'NONE', #16114, 1000.000000000000000 ) ;
#1548 = CIRCLE ( 'NONE', #8343, 6.000000000000001776 ) ;
#1549 = ORIENTED_EDGE ( 'NONE', *, *, #22549, .F. ) ;
#1550 = CIRCLE ( 'NONE', #22056, 35.00000000000000000 ) ;
#1551 = CARTESIAN_POINT ( 'NONE',  ( -26.59168384020000175, 38.48554521319999822, -140.5676127940000129 ) ) ;
#1552 = FACE_OUTER_BOUND ( 'NONE', #10090, .T. ) ;
#1553 = ORIENTED_EDGE ( 'NONE', *, *, #6685, .F. ) ;
#1554 = DIRECTION ( 'NONE',  ( 2.842170943040000002E-14, 3.552713678800000097E-13, 1.000000000000000000 ) ) ;
#1555 = ADVANCED_FACE ( 'NONE', ( #3374 ), #10615, .T. ) ;
#1556 = DIRECTION ( 'NONE',  ( 1.000000000000000000, 0.000000000000000000, -4.510774274160000731E-12 ) ) ;
#1557 = ORIENTED_EDGE ( 'NONE', *, *, #10489, .T. ) ;
#1558 = ADVANCED_FACE ( 'NONE', ( #3498 ), #8948, .F. ) ;
#1559 = CARTESIAN_POINT ( 'NONE',  ( -12.95309207270000051, 35.58606224190000233, -147.4460499719999689 ) ) ;
#1560 = EDGE_CURVE ( 'NONE', #16877, #6475, #54, .T. ) ;
#1561 = ADVANCED_FACE ( 'NONE', ( #23481 ), #16230, .T. ) ;
#1562 = ORIENTED_EDGE ( 'NONE', *, *, #14186, .T. ) ;
#1563 = AXIS2_PLACEMENT_3D ( 'NONE', #3226, #10458, #5121 ) ;
#1564 = AXIS2_PLACEMENT_3D ( 'NONE', #18973, #1265, #13968 ) ;
#1565 = CARTESIAN_POINT ( 'NONE',  ( -2.499999999859999988, 20.50000000000000000, -147.5552959529999839 ) ) ;
#1566 = CARTESIAN_POINT ( 'NONE',  ( 18.18320006080000084, -3.000000000000000000, -148.5552959529999839 ) ) ;
#1567 = CARTESIAN_POINT ( 'NONE',  ( -13.69605334181871115, 39.31347921127435541, -140.9805954651069158 ) ) ;
#1568 = CARTESIAN_POINT ( 'NONE',  ( -29.25462571399999590, 37.92445966660000778, -140.5403777589999947 ) ) ;
#1569 = ORIENTED_EDGE ( 'NONE', *, *, #5864, .T. ) ;
#1570 = CARTESIAN_POINT ( 'NONE',  ( 6.007375567817776485, 13.00000000000000533, -136.0552959530135695 ) ) ;
#1571 = CARTESIAN_POINT ( 'NONE',  ( -6.599319970649999867, -19.98386714700000155, -146.5552959529999839 ) ) ;
#1572 = PLANE ( 'NONE',  #22828 ) ;
#1573 = LINE ( 'NONE', #16187, #18169 ) ;
#1574 = DIRECTION ( 'NONE',  ( -0.9840552701943220404, 0.1778629393740580045, -3.651917849741195385E-14 ) ) ;
#1575 = CARTESIAN_POINT ( 'NONE',  ( -34.47299999999999898, 14.00000000000000000, -144.0552959529999839 ) ) ;
#1576 = ORIENTED_EDGE ( 'NONE', *, *, #7044, .F. ) ;
#1577 = SURFACE_STYLE_USAGE ( .BOTH. , #19998 ) ;
#1578 = CARTESIAN_POINT ( 'NONE',  ( 4.499999999879999102, -1.500000000000000000, -135.0552959530000123 ) ) ;
#1579 = CARTESIAN_POINT ( 'NONE',  ( 1.578081969995054568, -4.285243653077847270, -150.0552959530000123 ) ) ;
#1580 = CARTESIAN_POINT ( 'NONE',  ( -4.712143453930511150, 38.89658459788447686, -139.8814980668870760 ) ) ;
#1581 = CIRCLE ( 'NONE', #663, 1.499999999999996225 ) ;
#1582 = CARTESIAN_POINT ( 'NONE',  ( -23.71856152630000025, 38.62313066519999438, -140.3058339320000130 ) ) ;
#1583 = AXIS2_PLACEMENT_3D ( 'NONE', #11733, #4494, #6392 ) ;
#1584 = CARTESIAN_POINT ( 'NONE',  ( 18.95053822279999878, -50.00000000000000000, -150.5552959529999839 ) ) ;
#1585 = VECTOR ( 'NONE', #13004, 1000.000000000000000 ) ;
#1586 = ORIENTED_EDGE ( 'NONE', *, *, #10056, .F. ) ;
#1587 = CARTESIAN_POINT ( 'NONE',  ( 9.683200060759999062, -20.50000000000000000, -148.5552959529999839 ) ) ;
#1588 = EDGE_CURVE ( 'NONE', #2933, #20660, #20036, .T. ) ;
#1589 = DIRECTION ( 'NONE',  ( -1.211690350419999855E-27, -2.765629237170000203E-27, 1.000000000000000000 ) ) ;
#1590 = VERTEX_POINT ( 'NONE', #19566 ) ;
#1591 = CARTESIAN_POINT ( 'NONE',  ( -10.00000000000000000, 25.50000000000000000, -150.0552959529999839 ) ) ;
#1592 = ORIENTED_EDGE ( 'NONE', *, *, #20615, .F. ) ;
#1593 =( BOUNDED_CURVE ( )  B_SPLINE_CURVE ( 5, ( #12206, #14120, #17685, #2938, #22936, #10410, #4719, #3176, #10299, #21388, #5074, #8514 ),
 .UNSPECIFIED., .F., .F. ) 
 B_SPLINE_CURVE_WITH_KNOTS ( ( 6, 3, 3, 6 ),
 ( 0.000000000000000000, 4.059123295939999210, 8.340116530639999581, 12.86134770560000007 ),
 .UNSPECIFIED. ) 
 CURVE ( )  GEOMETRIC_REPRESENTATION_ITEM ( )  RATIONAL_B_SPLINE_CURVE ( ( 0.2500000000000000000, 0.2500000000000000000, 0.2500000000000000000, 0.2500000000000000000, 0.2500000000000000000, 0.2500000000000000000, 0.2500000000000000000, 0.2500000000000000000, 0.2500000000000000000, 0.2500000000000000000, 0.2500000000000000000, 0.2500000000000000000 ) ) 
 REPRESENTATION_ITEM ( '' )  );
#1594 = CARTESIAN_POINT ( 'NONE',  ( 3.999999999879999546, -1.500000000000000000, -135.4552959529999896 ) ) ;
#1595 = CARTESIAN_POINT ( 'NONE',  ( -29.25462571399999590, 37.92445966660000778, -140.5403777589999947 ) ) ;
#1596 = LINE ( 'NONE', #17523, #16597 ) ;
#1597 = CARTESIAN_POINT ( 'NONE',  ( 7.466903260932848951, 38.08760507689758157, -141.8042231706027394 ) ) ;
#1598 = ORIENTED_EDGE ( 'NONE', *, *, #2438, .F. ) ;
#1599 = CARTESIAN_POINT ( 'NONE',  ( -10.46662683120000104, 35.31824366040000029, -139.9138328150000063 ) ) ;
#1600 = AXIS2_PLACEMENT_3D ( 'NONE', #16675, #18813, #11188 ) ;
#1601 = CARTESIAN_POINT ( 'NONE',  ( -18.32340570184511463, 36.04493404334465367, -148.6528109212497952 ) ) ;
#1602 = AXIS2_PLACEMENT_3D ( 'NONE', #19669, #3608, #14558 ) ;
#1603 = CARTESIAN_POINT ( 'NONE',  ( -18.35824191589999899, -1.500000000000000000, -146.3157682189915931 ) ) ;
#1604 = FACE_OUTER_BOUND ( 'NONE', #8472, .T. ) ;
#1605 = ORIENTED_EDGE ( 'NONE', *, *, #1263, .T. ) ;
#1606 = CARTESIAN_POINT ( 'NONE',  ( 17.50006728700661540, 22.10251055748693005, -136.0552959530394901 ) ) ;
#1607 = SHAPE_REPRESENTATION_RELATIONSHIP ( 'NONE' , 'NONE' ,  #2821, #19731 ) ;
#1608 = ORIENTED_EDGE ( 'NONE', *, *, #1097, .T. ) ;
#1609 = FACE_OUTER_BOUND ( 'NONE', #5677, .T. ) ;
#1610 = CARTESIAN_POINT ( 'NONE',  ( -9.310255235759342440, -16.95797460217655939, -145.5552959530000692 ) ) ;
#1611 = DIRECTION ( 'NONE',  ( 1.000000000000000000, 0.000000000000000000, -4.429789868254373788E-12 ) ) ;
#1612 = ORIENTED_EDGE ( 'NONE', *, *, #20797, .T. ) ;
#1613 = EDGE_CURVE ( 'NONE', #5042, #7140, #17473, .T. ) ;
#1614 = CARTESIAN_POINT ( 'NONE',  ( 8.750000000000000000, -44.61803398880000060, -150.0552959529999839 ) ) ;
#1615 = CARTESIAN_POINT ( 'NONE',  ( 8.750000000030000891, -35.98606797749999942, -137.0552959530000123 ) ) ;
#1616 =( GEOMETRIC_REPRESENTATION_CONTEXT ( 3 ) GLOBAL_UNCERTAINTY_ASSIGNED_CONTEXT ( ( #16365 ) ) GLOBAL_UNIT_ASSIGNED_CONTEXT ( ( #10401, #21140, #19583 ) ) REPRESENTATION_CONTEXT ( 'NONE', 'WORKASPACE' ) );
#1617 = AXIS2_PLACEMENT_3D ( 'NONE', #9994, #22985, #17152 ) ;
#1618 = ORIENTED_EDGE ( 'NONE', *, *, #12855, .F. ) ;
#1619 = CIRCLE ( 'NONE', #13756, 6.000000000000001776 ) ;
#1620 = CARTESIAN_POINT ( 'NONE',  ( 0.5000000001590000354, 20.50000000000000000, -139.5552959529999839 ) ) ;
#1621 = CARTESIAN_POINT ( 'NONE',  ( 19.71940181154762328, 25.42378041200768379, -150.0552959530000123 ) ) ;
#1622 = CARTESIAN_POINT ( 'NONE',  ( -12.50000000000000000, 48.50000000000000000, -136.0552959530000123 ) ) ;
#1623 = DIRECTION ( 'NONE',  ( 1.000000000000000000, 0.000000000000000000, 2.516505522483685870E-12 ) ) ;
#1624 = DIRECTION ( 'NONE',  ( -0.6459422414661291079, -0.7633862853691523176, -2.273736754430455399E-12 ) ) ;
#1625 = CARTESIAN_POINT ( 'NONE',  ( -15.90559286389999905, 34.15404988380000617, -147.7469703310000000 ) ) ;
#1626 = CARTESIAN_POINT ( 'NONE',  ( 1.500000000000000000, -3.500000000000000000, -145.5552959529999839 ) ) ;
#1627 = CARTESIAN_POINT ( 'NONE',  ( -13.86630785140000022, 51.50000000000000000, -137.0552959530000123 ) ) ;
#1628 = DIRECTION ( 'NONE',  ( 0.000000000000000000, 1.000000000000000000, 0.000000000000000000 ) ) ;
#1629 = PRODUCT ( 'Faceplate Support', 'Faceplate Support', '', ( #5675 ) ) ;
#1630 = ORIENTED_EDGE ( 'NONE', *, *, #3766, .T. ) ;
#1631 = UNCERTAINTY_MEASURE_WITH_UNIT (LENGTH_MEASURE( 1.000000000000000082E-05 ), #2207, 'distance_accuracy_value', 'NONE');
#1632 = ORIENTED_EDGE ( 'NONE', *, *, #11313, .T. ) ;
#1633 = EDGE_LOOP ( 'NONE', ( #17440, #18528 ) ) ;
#1634 = DIRECTION ( 'NONE',  ( -1.457985068979999943E-12, -1.723073263340000007E-12, 1.000000000000000000 ) ) ;
#1635 = CARTESIAN_POINT ( 'NONE',  ( -28.04360111912153286, 34.66455527868549069, -140.6572026283309640 ) ) ;
#1636 = LINE ( 'NONE', #23390, #19437 ) ;
#1637 = DIRECTION ( 'NONE',  ( -1.000000000000000000, 0.000000000000000000, 0.000000000000000000 ) ) ;
#1638 = EDGE_LOOP ( 'NONE', ( #18762, #8978 ) ) ;
#1639 = EDGE_CURVE ( 'NONE', #8510, #12200, #10492, .T. ) ;
#1640 = DIRECTION ( 'NONE',  ( -0.06298685227120542907, -0.9980143568310855251, 1.534772309240130738E-13 ) ) ;
#1641 = CARTESIAN_POINT ( 'NONE',  ( -20.21101409811915772, 36.97743810397759745, -140.7155889590012237 ) ) ;
#1642 = CARTESIAN_POINT ( 'NONE',  ( -9.282104535849999394, -16.71402168319999859, -144.5552959529999839 ) ) ;
#1643 = EDGE_CURVE ( 'NONE', #4170, #6635, #15991, .T. ) ;
#1644 = CARTESIAN_POINT ( 'NONE',  ( 7.750000000030000002, -38.98606797749999942, -136.0552959530000123 ) ) ;
#1645 = ORIENTED_EDGE ( 'NONE', *, *, #18967, .F. ) ;
#1646 = CARTESIAN_POINT ( 'NONE',  ( -3.499999999959999997, 44.50000000000000000, -136.0552959530000123 ) ) ;
#1647 = ORIENTED_EDGE ( 'NONE', *, *, #21592, .F. ) ;
#1648 = CARTESIAN_POINT ( 'NONE',  ( 9.738534063751803416, 36.15378715822735955, -141.7028596377058705 ) ) ;
#1649 = AXIS2_PLACEMENT_3D ( 'NONE', #5854, #4424, #17156 ) ;
#1650 = DIRECTION ( 'NONE',  ( -0.000000000000000000, 1.000000000000000000, 0.000000000000000000 ) ) ;
#1651 = DIRECTION ( 'NONE',  ( 0.000000000000000000, 2.256894259919999967E-12, 1.000000000000000000 ) ) ;
#1652 = EDGE_LOOP ( 'NONE', ( #22705, #449, #5626, #4466, #23537, #11215 ) ) ;
#1653 = CYLINDRICAL_SURFACE ( 'NONE', #14492, 2.000000000000001776 ) ;
#1654 = ORIENTED_EDGE ( 'NONE', *, *, #574, .F. ) ;
#1655 = CARTESIAN_POINT ( 'NONE',  ( -18.48412402389261544, 36.99547888839300214, -147.4161207264765778 ) ) ;
#1656 = DIRECTION ( 'NONE',  ( 2.257157423930000049E-12, 0.000000000000000000, 1.000000000000000000 ) ) ;
#1657 = VERTEX_POINT ( 'NONE', #8323 ) ;
#1658 = CARTESIAN_POINT ( 'NONE',  ( -6.599319970649999867, -19.98386714700000155, -146.5552959529999839 ) ) ;
#1659 = VERTEX_POINT ( 'NONE', #21314 ) ;
#1660 = CARTESIAN_POINT ( 'NONE',  ( -15.57786843150000067, 37.00666880280000726, -148.5521201120000114 ) ) ;
#1661 = DIRECTION ( 'NONE',  ( 0.000000000000000000, -4.148443855749999753E-27, -1.000000000000000000 ) ) ;
#1662 = AXIS2_PLACEMENT_3D ( 'NONE', #3554, #1778, #21411 ) ;
#1663 = ORIENTED_EDGE ( 'NONE', *, *, #22844, .F. ) ;
#1664 = CARTESIAN_POINT ( 'NONE',  ( 0.000000000000000000, 0.000000000000000000, 0.000000000000000000 ) ) ;
#1665 = ORIENTED_EDGE ( 'NONE', *, *, #21182, .F. ) ;
#1666 = CARTESIAN_POINT ( 'NONE',  ( -27.04496201379999931, 40.71797592360000095, -143.5957174049999878 ) ) ;
#1667 = CARTESIAN_POINT ( 'NONE',  ( -38.72222222220000276, 46.25000000000000000, -140.5552959529999839 ) ) ;
#1668 = ORIENTED_EDGE ( 'NONE', *, *, #14006, .F. ) ;
#1669 = EDGE_CURVE ( 'NONE', #13712, #5167, #17729, .T. ) ;
#1670 = CARTESIAN_POINT ( 'NONE',  ( 24.55924402540000173, -29.20875385929999979, -142.5552959529999839 ) ) ;
#1671 = CARTESIAN_POINT ( 'NONE',  ( 20.50000000000000000, 25.50000000000000000, -136.5552959530000123 ) ) ;
#1672 = DIRECTION ( 'NONE',  ( 1.337196879809910072E-12, 0.000000000000000000, -1.000000000000000000 ) ) ;
#1673 = ORIENTED_EDGE ( 'NONE', *, *, #5958, .F. ) ;
#1674 = CARTESIAN_POINT ( 'NONE',  ( 5.347956485829999274, -22.34165470570000167, -146.5552959529999839 ) ) ;
#1675 = EDGE_CURVE ( 'NONE', #7250, #3831, #15948, .T. ) ;
#1676 = CARTESIAN_POINT ( 'NONE',  ( -13.21931118290000029, 33.83281470429999871, -146.0365350580000268 ) ) ;
#1677 = ORIENTED_EDGE ( 'NONE', *, *, #8212, .T. ) ;
#1678 = DIRECTION ( 'NONE',  ( -1.000000000000000000, 0.000000000000000000, 2.257171095940000041E-12 ) ) ;
#1679 = CARTESIAN_POINT ( 'NONE',  ( -11.26413364438170106, 36.97109742516077802, -139.4278719022366317 ) ) ;
#1680 = CARTESIAN_POINT ( 'NONE',  ( -14.35287446704815473, 40.57630474357829797, -143.6962090187504373 ) ) ;
#1681 = DIRECTION ( 'NONE',  ( -0.1000233216789610108, -0.9949850929136109245, 3.591470555298595137E-13 ) ) ;
#1682 = ORIENTED_EDGE ( 'NONE', *, *, #2724, .F. ) ;
#1683 = CARTESIAN_POINT ( 'NONE',  ( -0.6176558849126000394, 18.08432684250925959, -136.0552959529985628 ) ) ;
#1684 = DIRECTION ( 'NONE',  ( -1.000000000000000000, 0.000000000000000000, 2.257221436789999912E-12 ) ) ;
#1685 = ADVANCED_FACE ( 'NONE', ( #1329 ), #6779, .T. ) ;
#1686 = CARTESIAN_POINT ( 'NONE',  ( -9.282104535860000283, -16.71402168319999859, -145.5552959529999839 ) ) ;
#1687 = FACE_OUTER_BOUND ( 'NONE', #3541, .T. ) ;
#1688 = PLANE ( 'NONE',  #13621 ) ;
#1689 = EDGE_CURVE ( 'NONE', #2706, #23117, #19526, .T. ) ;
#1690 = ORIENTED_EDGE ( 'NONE', *, *, #8351, .T. ) ;
#1691 = CARTESIAN_POINT ( 'NONE',  ( -6.083910486889999802, -15.16899799649999991, -145.0552959529999839 ) ) ;
#1692 = ADVANCED_FACE ( 'NONE', ( #6899 ), #14167, .F. ) ;
#1693 = CARTESIAN_POINT ( 'NONE',  ( -3.499999999969999998, 40.00000000000000000, -137.0552959530000123 ) ) ;
#1694 = LINE ( 'NONE', #9027, #12502 ) ;
#1695 = EDGE_CURVE ( 'NONE', #8517, #8429, #19003, .T. ) ;
#1696 = CARTESIAN_POINT ( 'NONE',  ( -5.475508280718690557, 38.87484624601071914, -139.7033240574601223 ) ) ;
#1697 = DIRECTION ( 'NONE',  ( -1.000000000000000000, 0.000000000000000000, 0.000000000000000000 ) ) ;
#1698 = ORIENTED_EDGE ( 'NONE', *, *, #12513, .T. ) ;
#1699 = VECTOR ( 'NONE', #13346, 1000.000000000000000 ) ;
#1700 = CARTESIAN_POINT ( 'NONE',  ( 10.55105919799721192, -21.49999999999999289, -148.5552959529999839 ) ) ;
#1701 = CARTESIAN_POINT ( 'NONE',  ( -15.46613156839999981, 36.99333119719999985, -147.5584717940000132 ) ) ;
#1702 = ORIENTED_EDGE ( 'NONE', *, *, #11680, .T. ) ;
#1703 = ADVANCED_FACE ( 'NONE', ( #5115 ), #23091, .T. ) ;
#1704 = CARTESIAN_POINT ( 'NONE',  ( -24.06602356359999817, 36.94557182220000158, -148.2530914610000252 ) ) ;
#1705 = VERTEX_POINT ( 'NONE', #1444 ) ;
#1706 = CARTESIAN_POINT ( 'NONE',  ( -24.87949572109999963, 37.83967983510000010, -147.8465544160000036 ) ) ;
#1707 = CARTESIAN_POINT ( 'NONE',  ( -29.64895016830000429, 40.48034887659999725, -142.7934167989999992 ) ) ;
#1708 = CARTESIAN_POINT ( 'NONE',  ( 1.352544480119999948, -20.86379603889999856, -146.0552959529999839 ) ) ;
#1709 = CARTESIAN_POINT ( 'NONE',  ( 7.719632372826509048, 38.28109096042884119, -141.9084521925880154 ) ) ;
#1710 = ORIENTED_EDGE ( 'NONE', *, *, #9734, .T. ) ;
#1711 = PRESENTATION_STYLE_ASSIGNMENT (( #1825 ) ) ;
#1712 = CARTESIAN_POINT ( 'NONE',  ( -19.70924662384209824, 34.96809591615225088, -139.6648745877703846 ) ) ;
#1713 = ADVANCED_FACE ( 'NONE', ( #9986 ), #15826, .T. ) ;
#1714 = CARTESIAN_POINT ( 'NONE',  ( -9.483015687316079578, 40.53201449268256340, -146.0034198473055937 ) ) ;
#1715 = CARTESIAN_POINT ( 'NONE',  ( 9.593637377617811879, -34.75248504027396024, -136.0552959530216413 ) ) ;
#1716 = VECTOR ( 'NONE', #14645, 1000.000000000000000 ) ;
#1717 = VERTEX_POINT ( 'NONE', #19163 ) ;
#1718 = EDGE_CURVE ( 'NONE', #3899, #19035, #971, .T. ) ;
#1719 = DIRECTION ( 'NONE',  ( 0.000000000000000000, 0.000000000000000000, 1.000000000000000000 ) ) ;
#1720 =( LENGTH_UNIT ( ) NAMED_UNIT ( * ) SI_UNIT ( .MILLI., .METRE. ) );
#1721 = EDGE_CURVE ( 'NONE', #9450, #15840, #16517, .T. ) ;
#1722 = ORIENTED_EDGE ( 'NONE', *, *, #4603, .T. ) ;
#1723 = DIRECTION ( 'NONE',  ( -1.000000000000000000, 1.734728570689999873E-18, 2.257171095940000041E-12 ) ) ;
#1724 = FACE_OUTER_BOUND ( 'NONE', #16487, .T. ) ;
#1725 = CARTESIAN_POINT ( 'NONE',  ( -5.660514123294832167, 20.09808825513981034, -136.0552959529872510 ) ) ;
#1726 = ORIENTED_EDGE ( 'NONE', *, *, #22913, .F. ) ;
#1727 = CARTESIAN_POINT ( 'NONE',  ( -5.459597139462840865, 36.94776568914183912, -139.8191173758248169 ) ) ;
#1728 = CARTESIAN_POINT ( 'NONE',  ( 13.13369214870000157, -50.50000000000000000, -136.0552959530000123 ) ) ;
#1729 = ORIENTED_EDGE ( 'NONE', *, *, #12566, .T. ) ;
#1730 = DIRECTION ( 'NONE',  ( 1.000000000000000000, 0.000000000000000000, -8.955190032050000935E-12 ) ) ;
#1731 = CARTESIAN_POINT ( 'NONE',  ( 18.09808825512843455, 20.66051412331523451, -150.0552959529999839 ) ) ;
#1733 = AXIS2_PLACEMENT_3D ( 'NONE', #18267, #7423, #1856 ) ;
#1732 = LINE ( 'NONE', #16574, #20010 ) ;
#1734 = LINE ( 'NONE', #12531, #20139 ) ;
#1735 = DIRECTION ( 'NONE',  ( 2.256861364460000137E-12, 0.000000000000000000, 1.000000000000000000 ) ) ;
#1736 = CARTESIAN_POINT ( 'NONE',  ( 31.50000000000000000, -33.03620104880000241, -136.0552959530000123 ) ) ;
#1737 = DIRECTION ( 'NONE',  ( 1.000000000000000000, 0.000000000000000000, 2.516505522483685870E-12 ) ) ;
#1738 = LINE ( 'NONE', #1275, #12013 ) ;
#1739 = ADVANCED_FACE ( 'NONE', ( #22976 ), #6661, .F. ) ;
#1740 = DIRECTION ( 'NONE',  ( -2.257144641399999941E-12, 0.000000000000000000, -1.000000000000000000 ) ) ;
#1741 = EDGE_LOOP ( 'NONE', ( #373, #5143, #19981, #17412 ) ) ;
#1742 = EDGE_CURVE ( 'NONE', #3932, #15560, #19408, .T. ) ;
#1743 = EDGE_LOOP ( 'NONE', ( #18864, #2469, #148, #16701 ) ) ;
#1744 = ORIENTED_EDGE ( 'NONE', *, *, #18092, .T. ) ;
#1745 = CIRCLE ( 'NONE', #10058, 1.500000000000001332 ) ;
#1746 = DIRECTION ( 'NONE',  ( 0.000000000000000000, 6.069065783950000909E-29, -1.000000000000000000 ) ) ;
#1747 = CARTESIAN_POINT ( 'NONE',  ( -13.30167158631291358, 35.54685148874143863, -147.6446058646477013 ) ) ;
#1748 = CARTESIAN_POINT ( 'NONE',  ( 15.50000000000000000, 33.50000000000000000, -150.5552959529999839 ) ) ;
#1749 = AXIS2_PLACEMENT_3D ( 'NONE', #16844, #11581, #15406 ) ;
#1750 = DIRECTION ( 'NONE',  ( 0.000000000000000000, 0.000000000000000000, 1.000000000000000000 ) ) ;
#1751 = EDGE_LOOP ( 'NONE', ( #7956, #16364 ) ) ;
#1752 = CARTESIAN_POINT ( 'NONE',  ( -4.500000000000000000, 37.00000000000000000, -150.0552959529999839 ) ) ;
#1753 = CARTESIAN_POINT ( 'NONE',  ( -21.35824191589999899, -32.00000000000000000, -141.0657682190000060 ) ) ;
#1754 = CARTESIAN_POINT ( 'NONE',  ( -11.99109128264890423, 36.93662743998119424, -148.3295785879899427 ) ) ;
#1755 = FACE_OUTER_BOUND ( 'NONE', #6923, .T. ) ;
#1756 = VERTEX_POINT ( 'NONE', #20111 ) ;
#1757 = FACE_BOUND ( 'NONE', #16609, .T. ) ;
#1758 = EDGE_LOOP ( 'NONE', ( #23285, #13392 ) ) ;
#1759 = CARTESIAN_POINT ( 'NONE',  ( 9.297187311559401479, 35.72924951987560149, -141.9023098457803940 ) ) ;
#1760 = CARTESIAN_POINT ( 'NONE',  ( -31.50000000000000000, 19.50000000000000000, -143.3052959529999839 ) ) ;
#1761 = AXIS2_PLACEMENT_3D ( 'NONE', #2604, #7594, #9833 ) ;
#1762 = CARTESIAN_POINT ( 'NONE',  ( 10.68320006080000084, -20.50000000000000000, -148.5552959529999839 ) ) ;
#1763 = VECTOR ( 'NONE', #6573, 1000.000000000000000 ) ;
#1764 = EDGE_LOOP ( 'NONE', ( #7838, #22300, #568, #5436, #6540, #6553, #20066, #16969, #22280, #14198, #5137, #4958, #14790, #3028, #111 ) ) ;
#1765 = ADVANCED_FACE ( 'NONE', ( #11049 ), #18207, .T. ) ;
#1766 = EDGE_CURVE ( 'NONE', #14876, #5894, #19763, .T. ) ;
#1767 = FACE_OUTER_BOUND ( 'NONE', #16448, .T. ) ;
#1768 = ORIENTED_EDGE ( 'NONE', *, *, #5585, .F. ) ;
#1769 = CARTESIAN_POINT ( 'NONE',  ( -20.08037650829999876, 40.50744741009999927, -142.1449807700000179 ) ) ;
#1770 = EDGE_CURVE ( 'NONE', #4685, #18991, #9262, .T. ) ;
#1771 = DIRECTION ( 'NONE',  ( 3.994014902981375509E-29, -1.000000000000000000, 4.148443855750374987E-27 ) ) ;
#1772 = ORIENTED_EDGE ( 'NONE', *, *, #22316, .F. ) ;
#1773 = FACE_OUTER_BOUND ( 'NONE', #8786, .T. ) ;
#1774 = ORIENTED_EDGE ( 'NONE', *, *, #4121, .F. ) ;
#1775 = CARTESIAN_POINT ( 'NONE',  ( -21.73420140653708543, 36.02043114307134175, -148.7219678492595278 ) ) ;
#1776 = CARTESIAN_POINT ( 'NONE',  ( -5.449266527207747401, 43.97928331370365385, -150.0552959530000123 ) ) ;
#1777 = ORIENTED_EDGE ( 'NONE', *, *, #15799, .T. ) ;
#1778 = DIRECTION ( 'NONE',  ( 0.000000000000000000, 0.000000000000000000, 1.000000000000000000 ) ) ;
#1779 = VERTEX_POINT ( 'NONE', #7375 ) ;
#1780 = AXIS2_PLACEMENT_3D ( 'NONE', #5327, #3659, #9112 ) ;
#1781 = LINE ( 'NONE', #7356, #21776 ) ;
#1782 = ORIENTED_EDGE ( 'NONE', *, *, #3711, .T. ) ;
#1783 = AXIS2_PLACEMENT_3D ( 'NONE', #3514, #16004, #3050 ) ;
#1784 = DIRECTION ( 'NONE',  ( 2.839308199624610116E-14, 3.568879590629954805E-13, 1.000000000000000000 ) ) ;
#1785 = DIRECTION ( 'NONE',  ( 4.430318231639999944E-12, -6.100259101500000139E-13, 1.000000000000000000 ) ) ;
#1786 = CARTESIAN_POINT ( 'NONE',  ( 8.750000000000000000, -38.23606797749999942, -151.0552959529999839 ) ) ;
#1787 = EDGE_LOOP ( 'NONE', ( #4671, #15389, #22325, #20050 ) ) ;
#1788 = CARTESIAN_POINT ( 'NONE',  ( -2.499999999839999987, 41.50000000000000000, -140.0552959529999839 ) ) ;
#1789 = ORIENTED_EDGE ( 'NONE', *, *, #10649, .F. ) ;
#1790 = DIRECTION ( 'NONE',  ( -2.257171095940000041E-12, -1.003664318210000046E-28, -1.000000000000000000 ) ) ;
#1791 = PLANE ( 'NONE',  #4808 ) ;
#1792 = FACE_BOUND ( 'NONE', #9087, .T. ) ;
#1793 = DIRECTION ( 'NONE',  ( 0.000000000000000000, -1.000000000000000000, 0.000000000000000000 ) ) ;
#1794 = VECTOR ( 'NONE', #22122, 1000.000000000000000 ) ;
#1795 = EDGE_LOOP ( 'NONE', ( #13048, #3731 ) ) ;
#1796 = CARTESIAN_POINT ( 'NONE',  ( -31.00000000000000000, 47.50000000000000000, -149.5552959529999839 ) ) ;
#1797 = EDGE_CURVE ( 'NONE', #322, #7233, #14526, .T. ) ;
#1798 = LINE ( 'NONE', #11048, #11607 ) ;
#1799 = CARTESIAN_POINT ( 'NONE',  ( 32.50000000000000000, -39.80430157320000006, -149.5552959529999839 ) ) ;
#1800 = CARTESIAN_POINT ( 'NONE',  ( -9.434278515689999978, -18.41834002140000237, -146.5552959529999839 ) ) ;
#1801 = CARTESIAN_POINT ( 'NONE',  ( 29.68320006080000084, -32.50000000000000000, -148.5552959529999839 ) ) ;
#1802 = DIRECTION ( 'NONE',  ( 1.000000000000000000, 0.000000000000000000, -1.527536832333223921E-13 ) ) ;
#1803 = EDGE_LOOP ( 'NONE', ( #22187, #5500, #20182, #8623 ) ) ;
#1804 = DIRECTION ( 'NONE',  ( 2.257157423930000049E-12, 0.000000000000000000, 1.000000000000000000 ) ) ;
#1805 = PRODUCT_DEFINITION ( 'UNKNOWN', '', #21032, #4949 ) ;
#1806 = LINE ( 'NONE', #14287, #7614 ) ;
#1807 = CARTESIAN_POINT ( 'NONE',  ( 7.421918030004952094, -4.285243653077828618, -150.0552959530000123 ) ) ;
#1808 = ADVANCED_FACE ( 'NONE', ( #3812, #21902, #18327, #16533, #12834, #3331, #1924, #17854, #2039 ), #1572, .F. ) ;
#1809 = CARTESIAN_POINT ( 'NONE',  ( -6.397971003482101793, 41.16484389488864792, -146.3678220594143795 ) ) ;
#1810 = DIRECTION ( 'NONE',  ( 0.000000000000000000, -1.000000000000000000, 3.568879590630000244E-13 ) ) ;
#1811 = CIRCLE ( 'NONE', #15854, 0.5000000000000004441 ) ;
#1812 = ORIENTED_EDGE ( 'NONE', *, *, #10380, .T. ) ;
#1813 = CARTESIAN_POINT ( 'NONE',  ( 9.810832519885522629, -21.00613386075831457, -148.5552959529999839 ) ) ;
#1814 = VECTOR ( 'NONE', #10597, 1000.000000000000000 ) ;
#1815 = CARTESIAN_POINT ( 'NONE',  ( -32.50000000000000000, -51.50000000000000000, -149.5552959519999945 ) ) ;
#1816 = ORIENTED_EDGE ( 'NONE', *, *, #23431, .T. ) ;
#1817 = ADVANCED_FACE ( 'NONE', ( #9019 ), #10924, .F. ) ;
#1818 = CARTESIAN_POINT ( 'NONE',  ( -24.97797643630000053, 37.05442817780000553, -147.8575004449999994 ) ) ;
#1819 = ORIENTED_EDGE ( 'NONE', *, *, #16781, .T. ) ;
#1820 = CARTESIAN_POINT ( 'NONE',  ( -23.86695901012427967, 38.68196870791431508, -148.0474502905817928 ) ) ;
#1821 = CARTESIAN_POINT ( 'NONE',  ( -30.15470591354345586, 40.57106738518383082, -144.2503661066654956 ) ) ;
#1822 = LINE ( 'NONE', #14771, #2195 ) ;
#1823 = CARTESIAN_POINT ( 'NONE',  ( 7.879765099526474081, 38.36639659745271302, -141.9617131063228328 ) ) ;
#1824 = ORIENTED_EDGE ( 'NONE', *, *, #17504, .F. ) ;
#1825 = SURFACE_STYLE_USAGE ( .BOTH. , #20020 ) ;
#1826 = EDGE_CURVE ( 'NONE', #18313, #11439, #12479, .T. ) ;
#1827 = CARTESIAN_POINT ( 'NONE',  ( -18.86860405549940012, 33.24829707042102456, -142.0020245836044239 ) ) ;
#1828 = AXIS2_PLACEMENT_3D ( 'NONE', #8316, #5953, #13686 ) ;
#1829 = CARTESIAN_POINT ( 'NONE',  ( -9.971101149792001905, 37.05360750094371980, -147.8421425034861727 ) ) ;
#1830 = CARTESIAN_POINT ( 'NONE',  ( 9.167789811918616749, -35.55184220689274355, -136.0552959530206749 ) ) ;
#1831 = ORIENTED_EDGE ( 'NONE', *, *, #19563, .T. ) ;
#1832 = VECTOR ( 'NONE', #10189, 1000.000000000000000 ) ;
#1833 = DIRECTION ( 'NONE',  ( 0.000000000000000000, 0.000000000000000000, 1.000000000000000000 ) ) ;
#1834 = EDGE_CURVE ( 'NONE', #11473, #21810, #8790, .T. ) ;
#1835 = EDGE_LOOP ( 'NONE', ( #19495, #20776, #3199, #14764 ) ) ;
#1836 = CARTESIAN_POINT ( 'NONE',  ( 31.82297112080000190, 40.41789419139999495, -149.5552959529999839 ) ) ;
#1837 = EDGE_CURVE ( 'NONE', #576, #1513, #10267, .T. ) ;
#1838 = DIRECTION ( 'NONE',  ( 1.000000000000000000, 0.000000000000000000, 2.507771768019999718E-12 ) ) ;
#1839 = DIRECTION ( 'NONE',  ( 0.000000000000000000, -1.000000000000000000, 8.159623473500000156E-13 ) ) ;
#1840 = EDGE_LOOP ( 'NONE', ( #12851, #21123, #11960, #23063 ) ) ;
#1841 = FACE_OUTER_BOUND ( 'NONE', #9955, .T. ) ;
#1842 = DIRECTION ( 'NONE',  ( 0.000000000000000000, 1.000000000000000000, 0.000000000000000000 ) ) ;
#1843 = ORIENTED_EDGE ( 'NONE', *, *, #22120, .T. ) ;
#1844 = VECTOR ( 'NONE', #23210, 1000.000000000000000 ) ;
#1845 = ADVANCED_FACE ( 'NONE', ( #19881 ), #12932, .T. ) ;
#1846 = PLANE ( 'NONE',  #21250 ) ;
#1847 = EDGE_CURVE ( 'NONE', #21627, #4947, #18646, .T. ) ;
#1848 = VECTOR ( 'NONE', #10158, 1000.000000000000000 ) ;
#1849 = LINE ( 'NONE', #20040, #1010 ) ;
#1850 = DIRECTION ( 'NONE',  ( -1.000000000000000000, 0.000000000000000000, 2.257120985840000117E-12 ) ) ;
#1851 = ADVANCED_FACE ( 'NONE', ( #17975 ), #16305, .F. ) ;
#1852 = CARTESIAN_POINT ( 'NONE',  ( 32.14594224149999491, 40.79958733410000349, -142.8052959529999839 ) ) ;
#1853 = EDGE_CURVE ( 'NONE', #16606, #15863, #6856, .T. ) ;
#1854 = CARTESIAN_POINT ( 'NONE',  ( 19.59648046430000079, -50.76338628540000286, -149.5552959529999839 ) ) ;
#1855 = CARTESIAN_POINT ( 'NONE',  ( 3.999999999879999546, -4.750000000000000000, -135.4552959529999896 ) ) ;
#1856 = DIRECTION ( 'NONE',  ( 0.000000000000000000, -0.7071067811870332953, 0.7071067811860618502 ) ) ;
#1857 = CARTESIAN_POINT ( 'NONE',  ( -3.499999999959999997, 42.50000000000000000, -136.0552959530000123 ) ) ;
#1858 = ORIENTED_EDGE ( 'NONE', *, *, #21584, .T. ) ;
#1859 = UNCERTAINTY_MEASURE_WITH_UNIT (LENGTH_MEASURE( 1.000000000000000082E-05 ), #20777, 'distance_accuracy_value', 'NONE');
#1861 = VERTEX_POINT ( 'NONE', #21673 ) ;
#1860 = AXIS2_PLACEMENT_3D ( 'NONE', #4174, #13436, #6191 ) ;
#1862 = CIRCLE ( 'NONE', #9426, 2.999999999999999112 ) ;
#1863 = VERTEX_POINT ( 'NONE', #1799 ) ;
#1864 = DIRECTION ( 'NONE',  ( 0.000000000000000000, 1.000000000000000000, 0.000000000000000000 ) ) ;
#1865 = CARTESIAN_POINT ( 'NONE',  ( -12.86016529610566117, 36.30837334279895146, -147.6243440205185777 ) ) ;
#1866 = ORIENTED_EDGE ( 'NONE', *, *, #3854, .T. ) ;
#1867 = DIRECTION ( 'NONE',  ( 4.500711553433139826E-12, 0.000000000000000000, 1.000000000000000000 ) ) ;
#1868 = ORIENTED_EDGE ( 'NONE', *, *, #5451, .T. ) ;
#1869 = DIRECTION ( 'NONE',  ( 0.000000000000000000, 0.000000000000000000, 1.000000000000000000 ) ) ;
#1870 = CARTESIAN_POINT ( 'NONE',  ( -19.50275481447760484, 33.54643882699141244, -144.6274805566119426 ) ) ;
#1871 = CARTESIAN_POINT ( 'NONE',  ( -11.57042140271139985, 39.24233794802490394, -147.3928844070919126 ) ) ;
#1872 = DIRECTION ( 'NONE',  ( 0.6459422414661299960, -0.7633862853691516515, 0.000000000000000000 ) ) ;
#1873 = ORIENTED_EDGE ( 'NONE', *, *, #12997, .F. ) ;
#1874 = DIRECTION ( 'NONE',  ( 0.9934078757590584230, -0.1146332952500066366, -4.471042303700262431E-12 ) ) ;
#1875 = ADVANCED_BREP_SHAPE_REPRESENTATION ( '', ( #11538, #5025 ), #13402 ) ;
#1876 = ORIENTED_EDGE ( 'NONE', *, *, #7732, .F. ) ;
#1877 = CARTESIAN_POINT ( 'NONE',  ( 8.673959633207795505, 35.50990985248334653, -142.0478861723181581 ) ) ;
#1878 = EDGE_CURVE ( 'NONE', #23163, #683, #12, .T. ) ;
#1879 = CIRCLE ( 'NONE', #335, 2.000000000000000000 ) ;
#1880 = LINE ( 'NONE', #197, #5897 ) ;
#1881 = CIRCLE ( 'NONE', #14023, 7.499999999999999112 ) ;
#1882 = CARTESIAN_POINT ( 'NONE',  ( -31.50000000000000000, 19.50000000000000000, -137.0552959530000123 ) ) ;
#1883 = EDGE_LOOP ( 'NONE', ( #2656, #6930, #13439, #15350 ) ) ;
#1884 = AXIS2_PLACEMENT_3D ( 'NONE', #9269, #18337, #3821 ) ;
#1885 = AXIS2_PLACEMENT_3D ( 'NONE', #17176, #2446, #9900 ) ;
#1886 = LINE ( 'NONE', #7226, #2707 ) ;
#1887 = ORIENTED_EDGE ( 'NONE', *, *, #13153, .T. ) ;
#1888 = CARTESIAN_POINT ( 'NONE',  ( 20.50000000000000000, 25.50000000000000000, -136.0552959530000123 ) ) ;
#1889 = LINE ( 'NONE', #19608, #13521 ) ;
#1890 = ORIENTED_EDGE ( 'NONE', *, *, #12099, .F. ) ;
#1891 = CARTESIAN_POINT ( 'NONE',  ( -26.16983372450180312, 40.98399646778832306, -141.7700373849442030 ) ) ;
#1892 = VERTEX_POINT ( 'NONE', #14174 ) ;
#1893 = CARTESIAN_POINT ( 'NONE',  ( -22.14393879224838813, 35.16037992174653937, -148.2535502083404140 ) ) ;
#1894 = LINE ( 'NONE', #110, #16673 ) ;
#1895 = ORIENTED_EDGE ( 'NONE', *, *, #21508, .F. ) ;
#1896 = PRODUCT ( 'Slider', 'Slider', '', ( #14101 ) ) ;
#1897 = VECTOR ( 'NONE', #16751, 1000.000000000000000 ) ;
#1898 = ORIENTED_EDGE ( 'NONE', *, *, #12267, .T. ) ;
#1899 = CARTESIAN_POINT ( 'NONE',  ( -27.10979229004369628, 41.68302333980914653, -143.4785537008253868 ) ) ;
#1900 = AXIS2_PLACEMENT_3D ( 'NONE', #9741, #20831, #859 ) ;
#1901 = LINE ( 'NONE', #1667, #8045 ) ;
#1902 = ORIENTED_EDGE ( 'NONE', *, *, #14694, .F. ) ;
#1903 = DIRECTION ( 'NONE',  ( 2.257171095940000041E-12, 1.003664318210000046E-28, 1.000000000000000000 ) ) ;
#1904 = VECTOR ( 'NONE', #5881, 1000.000000000000000 ) ;
#1905 = CARTESIAN_POINT ( 'NONE',  ( -10.50683292394248092, 35.68768245788039906, -140.8109541216290950 ) ) ;
#1906 = EDGE_CURVE ( 'NONE', #3707, #18017, #5366, .T. ) ;
#1907 = CIRCLE ( 'NONE', #3053, 2.000000000000000888 ) ;
#1908 = LINE ( 'NONE', #21656, #19722 ) ;
#1909 = CIRCLE ( 'NONE', #8712, 8.176568160360000448 ) ;
#1910 = ORIENTED_EDGE ( 'NONE', *, *, #5021, .F. ) ;
#1911 = DIRECTION ( 'NONE',  ( 0.000000000000000000, -1.000000000000000000, 0.000000000000000000 ) ) ;
#1912 = LINE ( 'NONE', #11380, #10974 ) ;
#1913 = ORIENTED_EDGE ( 'NONE', *, *, #11237, .T. ) ;
#1914 = CARTESIAN_POINT ( 'NONE',  ( 7.750000000000000000, -42.23606797749999942, -150.0552959529999839 ) ) ;
#1915 = CARTESIAN_POINT ( 'NONE',  ( -2.499999999839999987, 31.00000000000000000, -139.5552959529999839 ) ) ;
#1916 = CARTESIAN_POINT ( 'NONE',  ( -15.07147389518837954, 36.94622240756218901, -147.6034838242705973 ) ) ;
#1917 = CARTESIAN_POINT ( 'NONE',  ( -29.82391180389999619, 40.55477172079999804, -144.2881336360000262 ) ) ;
#1918 = ORIENTED_EDGE ( 'NONE', *, *, #15768, .T. ) ;
#1919 = CARTESIAN_POINT ( 'NONE',  ( -15.00000000000000000, -41.50000000000000000, -136.0552959530000123 ) ) ;
#1920 = LINE ( 'NONE', #5476, #245 ) ;
#1921 = VECTOR ( 'NONE', #548, 1000.000000000000000 ) ;
#1922 = CIRCLE ( 'NONE', #6467, 5.999999999999998224 ) ;
#1923 = ADVANCED_FACE ( 'NONE', ( #14535 ), #18215, .F. ) ;
#1924 = FACE_BOUND ( 'NONE', #3093, .T. ) ;
#1925 = DIRECTION ( 'NONE',  ( 1.000000000000000000, 0.000000000000000000, -2.258609965721802837E-12 ) ) ;
#1926 = CARTESIAN_POINT ( 'NONE',  ( -32.50000000000000000, 48.00000000000000000, -146.5552959529999839 ) ) ;
#1927 = VECTOR ( 'NONE', #7417, 1000.000000000000000 ) ;
#1928 = CARTESIAN_POINT ( 'NONE',  ( 6.499999999879999102, -3.500000000000000000, -143.0552959529999839 ) ) ;
#1929 = CIRCLE ( 'NONE', #21679, 1.500000000000001332 ) ;
#1930 = ORIENTED_EDGE ( 'NONE', *, *, #5461, .T. ) ;
#1931 = DIRECTION ( 'NONE',  ( 0.000000000000000000, 1.000000000000000000, 0.000000000000000000 ) ) ;
#1932 = CARTESIAN_POINT ( 'NONE',  ( 10.38320006080000013, -24.50000000000000000, -150.0552959529999839 ) ) ;
#1933 = CARTESIAN_POINT ( 'NONE',  ( 1.878640834937229442, -5.010856941112704632, -150.0552959530000123 ) ) ;
#1934 = CARTESIAN_POINT ( 'NONE',  ( -5.762834418027599881, 39.50865942494267813, -140.4825946863184072 ) ) ;
#1935 = CARTESIAN_POINT ( 'NONE',  ( -13.50000000000000000, -43.00000000000000000, -136.0552959530000123 ) ) ;
#1936 = VERTEX_POINT ( 'NONE', #12615 ) ;
#1937 = ADVANCED_FACE ( 'NONE', ( #21437 ), #21798, .F. ) ;
#1938 = CARTESIAN_POINT ( 'NONE',  ( 10.42222808941079926, -21.47401663120255577, -148.5552959530000123 ) ) ;
#1939 = LINE ( 'NONE', #12738, #2614 ) ;
#1940 = EDGE_CURVE ( 'NONE', #15326, #12329, #5483, .T. ) ;
#1941 = ORIENTED_EDGE ( 'NONE', *, *, #3278, .T. ) ;
#1942 = AXIS2_PLACEMENT_3D ( 'NONE', #21792, #14397, #18087 ) ;
#1943 =( BOUNDED_CURVE ( )  B_SPLINE_CURVE ( 5, ( #12719, #14395, #20233, #11160, #7016, #3926 ),
 .UNSPECIFIED., .F., .F. ) 
 B_SPLINE_CURVE_WITH_KNOTS ( ( 6, 6 ),
 ( 1.570796327036584783, 3.141592653590000062 ),
 .UNSPECIFIED. ) 
 CURVE ( )  GEOMETRIC_REPRESENTATION_ITEM ( )  RATIONAL_B_SPLINE_CURVE ( ( 0.2500000000000000000, 0.2500000000307595616, 0.3000000000461393035, 0.4000000000615190898, 0.6000000000615191009, 1.000000000000000000 ) ) 
 REPRESENTATION_ITEM ( '' )  );
#1944 = DIRECTION ( 'NONE',  ( 1.000000000000000000, 0.000000000000000000, -2.253752739989067373E-12 ) ) ;
#1945 = EDGE_LOOP ( 'NONE', ( #12442, #20011, #19749, #3060, #2593, #7811, #4743, #18994, #314, #1569, #11789, #3631 ) ) ;
#1946 = CARTESIAN_POINT ( 'NONE',  ( -24.31357332192622778, 38.37299497772424672, -147.2056731264148084 ) ) ;
#1947 = DIRECTION ( 'NONE',  ( 0.000000000000000000, 1.000000000000000000, -2.245315044929999938E-12 ) ) ;
#1948 = LINE ( 'NONE', #3834, #4457 ) ;
#1949 = CARTESIAN_POINT ( 'NONE',  ( 3.611688725869999975E-11, 33.50000000000000000, -136.0552959530000123 ) ) ;
#1950 = ORIENTED_EDGE ( 'NONE', *, *, #3801, .F. ) ;
#1951 = DIRECTION ( 'NONE',  ( 1.000000000000000000, 2.004714280773594901E-17, -1.095180403012019938E-17 ) ) ;
#1952 = CARTESIAN_POINT ( 'NONE',  ( -19.18314309878111956, 35.27735355289885177, -140.1794542500113039 ) ) ;
#1953 = CARTESIAN_POINT ( 'NONE',  ( 2.218297500549999857, -15.44723318490000175, -147.5552959529999839 ) ) ;
#1954 = CARTESIAN_POINT ( 'NONE',  ( 9.479581287912614229, -35.03079462197541716, -136.0552959530214139 ) ) ;
#1955 = FACE_OUTER_BOUND ( 'NONE', #9695, .T. ) ;
#1956 = LINE ( 'NONE', #5619, #807 ) ;
#1957 = EDGE_CURVE ( 'NONE', #1276, #20629, #12257, .T. ) ;
#1958 = PLANE ( 'NONE',  #5768 ) ;
#1959 = LINE ( 'NONE', #274, #17162 ) ;
#1960 = CARTESIAN_POINT ( 'NONE',  ( -2.499999999859999988, 41.50000000000000000, -147.5552959529999839 ) ) ;
#1961 = ORIENTED_EDGE ( 'NONE', *, *, #19342, .T. ) ;
#1962 = CARTESIAN_POINT ( 'NONE',  ( -6.608289563844804704, 38.45937946434654009, -147.2295807508219525 ) ) ;
#1963 = EDGE_CURVE ( 'NONE', #10427, #4104, #7381, .T. ) ;
#1964 = ORIENTED_EDGE ( 'NONE', *, *, #14914, .F. ) ;
#1965 = FACE_OUTER_BOUND ( 'NONE', #13295, .T. ) ;
#1966 = DIRECTION ( 'NONE',  ( 0.9980143568310856361, -0.06298685227120542907, -4.509810669690387962E-12 ) ) ;
#1967 = LINE ( 'NONE', #18260, #3295 ) ;
#1968 = AXIS2_PLACEMENT_3D ( 'NONE', #10420, #17698, #15908 ) ;
#1969 = VECTOR ( 'NONE', #544, 1000.000000000000000 ) ;
#1970 = CARTESIAN_POINT ( 'NONE',  ( 4.750000000000000000, -42.61803398880000060, -150.0552959529999839 ) ) ;
#1971 = VECTOR ( 'NONE', #138, 1000.000000000000000 ) ;
#1972 = CARTESIAN_POINT ( 'NONE',  ( -13.86630785130000021, 50.50000000000000000, -137.0552959530000123 ) ) ;
#1973 = EDGE_CURVE ( 'NONE', #18574, #11235, #9120, .T. ) ;
#1974 = CARTESIAN_POINT ( 'NONE',  ( 19.68320006079999729, -20.50000000000000000, -150.0552959529999839 ) ) ;
#1975 = ITEM_DEFINED_TRANSFORMATION ( 'NONE', 'NONE', #1662,  #5025 ) ;
#1976 = CARTESIAN_POINT ( 'NONE',  ( -17.22605506639999717, 36.97564272059999979, -139.5994799229999899 ) ) ;
#1977 = LINE ( 'NONE', #14924, #8160 ) ;
#1978 = DIRECTION ( 'NONE',  ( -1.000000000000000000, -3.994014904670000134E-29, 2.423380700840000070E-27 ) ) ;
#1979 = ORIENTED_EDGE ( 'NONE', *, *, #20130, .T. ) ;
#1980 = ORIENTED_EDGE ( 'NONE', *, *, #3260, .F. ) ;
#1981 = FILL_AREA_STYLE_COLOUR ( '', #20998 ) ;
#1982 = EDGE_CURVE ( 'NONE', #3707, #10668, #19532, .T. ) ;
#1983 = EDGE_CURVE ( 'NONE', #23428, #9439, #1806, .T. ) ;
#1984 = ORIENTED_EDGE ( 'NONE', *, *, #6937, .F. ) ;
#1985 = CARTESIAN_POINT ( 'NONE',  ( -17.37032063983712860, 35.50980293810385291, -140.6805347145502196 ) ) ;
#1986 = DIRECTION ( 'NONE',  ( 0.5768293036180225375, -0.8168647100270319816, -3.053113317719179274E-12 ) ) ;
#1987 = ORIENTED_EDGE ( 'NONE', *, *, #13409, .T. ) ;
#1988 = VECTOR ( 'NONE', #12361, 1000.000000000000000 ) ;
#1989 = VECTOR ( 'NONE', #20619, 1000.000000000000000 ) ;
#1990 = CARTESIAN_POINT ( 'NONE',  ( 7.683200060759999950, -19.50000000000000000, -138.5552959529999839 ) ) ;
#1991 = VECTOR ( 'NONE', #3846, 1000.000000000000227 ) ;
#1992 = ADVANCED_FACE ( 'NONE', ( #15956 ), #10575, .T. ) ;
#1993 = ORIENTED_EDGE ( 'NONE', *, *, #14572, .F. ) ;
#1994 = CARTESIAN_POINT ( 'NONE',  ( 22.89800326577455181, 33.50000000000002132, -136.0552959530517683 ) ) ;
#1995 = EDGE_CURVE ( 'NONE', #8661, #7495, #22169, .T. ) ;
#1996 = CARTESIAN_POINT ( 'NONE',  ( -19.79103853767445287, 33.24264095657647999, -144.7076267160936140 ) ) ;
#1997 = DIRECTION ( 'NONE',  ( 0.7071067811865469066, -0.7071067811865481278, -1.591319668629387474E-12 ) ) ;
#1998 = VERTEX_POINT ( 'NONE', #16077 ) ;
#1999 = CARTESIAN_POINT ( 'NONE',  ( 6.500000000040000003, 13.00000000000000000, -136.0552959530000123 ) ) ;
#2000 = VERTEX_POINT ( 'NONE', #20000 ) ;
#2001 = CARTESIAN_POINT ( 'NONE',  ( 9.949375129378253746, 37.38976472558845643, -141.5855402290607685 ) ) ;
#2002 = LINE ( 'NONE', #1760, #15023 ) ;
#2003 = CARTESIAN_POINT ( 'NONE',  ( -28.00347998534502736, 37.05747243975537231, -148.5422211674043353 ) ) ;
#2004 = AXIS2_PLACEMENT_3D ( 'NONE', #20460, #3814, #4155 ) ;
#2005 = ORIENTED_EDGE ( 'NONE', *, *, #2166, .T. ) ;
#2006 = VECTOR ( 'NONE', #18307, 1000.000000000000227 ) ;
#2007 = VECTOR ( 'NONE', #9698, 1000.000000000000000 ) ;
#2008 = DIRECTION ( 'NONE',  ( 1.000000000000000000, 0.000000000000000000, -2.273736754470000126E-12 ) ) ;
#2009 = ORIENTED_EDGE ( 'NONE', *, *, #3205, .F. ) ;
#2010 = CARTESIAN_POINT ( 'NONE',  ( -4.499999999959999109, 34.00000000000000000, -153.0552959529999839 ) ) ;
#2011 = ORIENTED_EDGE ( 'NONE', *, *, #13892, .F. ) ;
#2012 = CARTESIAN_POINT ( 'NONE',  ( -25.58569844857837339, 38.74756584344044796, -140.2713792647305411 ) ) ;
#2013 = ADVANCED_FACE ( 'NONE', ( #19771, #23333 ), #3696, .T. ) ;
#2014 = VERTEX_POINT ( 'NONE', #1932 ) ;
#2015 = CARTESIAN_POINT ( 'NONE',  ( -22.71761275429354754, 35.08418826686737901, -139.6199258849947000 ) ) ;
#2016 = EDGE_CURVE ( 'NONE', #11959, #17690, #16433, .T. ) ;
#2017 = DIRECTION ( 'NONE',  ( -2.602084747549999882E-17, 1.000000000000000000, 5.873289694040000105E-29 ) ) ;
#2018 = ORIENTED_EDGE ( 'NONE', *, *, #12624, .T. ) ;
#2019 = PRODUCT_CONTEXT ( 'NONE', #20893, 'mechanical' ) ;
#2020 = ORIENTED_EDGE ( 'NONE', *, *, #18687, .T. ) ;
#2021 = FACE_OUTER_BOUND ( 'NONE', #591, .T. ) ;
#2022 = LINE ( 'NONE', #3228, #4549 ) ;
#2023 = DIRECTION ( 'NONE',  ( 0.000000000000000000, 0.000000000000000000, 1.000000000000000000 ) ) ;
#2024 = DIRECTION ( 'NONE',  ( -2.257242012349999735E-12, 0.000000000000000000, 1.000000000000000000 ) ) ;
#2025 = VECTOR ( 'NONE', #8459, 1000.000000000000000 ) ;
#2026 = CARTESIAN_POINT ( 'NONE',  ( -10.46662683120000104, 35.31824366040000029, -139.9138328150000063 ) ) ;
#2027 = CARTESIAN_POINT ( 'NONE',  ( 19.84954298779999959, 51.20423285649999912, -150.0552959529999839 ) ) ;
#2028 = VERTEX_POINT ( 'NONE', #14642 ) ;
#2029 = CARTESIAN_POINT ( 'NONE',  ( -12.86016529629999994, 36.30837334279999595, -147.6243440209999847 ) ) ;
#2030 = CARTESIAN_POINT ( 'NONE',  ( 18.95053822279999878, 50.00000000000000000, -149.5552959529999839 ) ) ;
#2031 = VERTEX_POINT ( 'NONE', #14406 ) ;
#2032 = DIRECTION ( 'NONE',  ( -0.1146332952500066227, -0.9934078757590583120, -9.710750722050572275E-14 ) ) ;
#2033 = DIRECTION ( 'NONE',  ( 1.000000000000000000, 0.000000000000000000, 0.000000000000000000 ) ) ;
#2034 = DIRECTION ( 'NONE',  ( 1.000000000000000000, 0.000000000000000000, -2.257144641399999941E-12 ) ) ;
#2035 = LINE ( 'NONE', #9364, #6058 ) ;
#2036 = ORIENTED_EDGE ( 'NONE', *, *, #4437, .F. ) ;
#2037 = CARTESIAN_POINT ( 'NONE',  ( 31.50000000000000000, -33.03620104880000241, -136.5552959530000123 ) ) ;
#2038 = DIRECTION ( 'NONE',  ( -0.07970438983373200059, -0.9968185442904001770, 8.268133652483321323E-13 ) ) ;
#2039 = FACE_OUTER_BOUND ( 'NONE', #4407, .T. ) ;
#2040 = DIRECTION ( 'NONE',  ( 1.000000000000000000, 0.000000000000000000, 0.000000000000000000 ) ) ;
#2041 = FACE_OUTER_BOUND ( 'NONE', #13396, .T. ) ;
#2042 = ADVANCED_FACE ( 'NONE', ( #23216 ), #16888, .F. ) ;
#2043 = DIRECTION ( 'NONE',  ( 0.9980719161006958995, 0.06206811009758109871, -2.049912714059374948E-13 ) ) ;
#2044 = EDGE_CURVE ( 'NONE', #6018, #11453, #249, .T. ) ;
#2045 = VERTEX_POINT ( 'NONE', #22138 ) ;
#2046 = LINE ( 'NONE', #7831, #12595 ) ;
#2047 = CARTESIAN_POINT ( 'NONE',  ( 20.31210873290000052, -31.32069079449999904, -146.5552959529999839 ) ) ;
#2048 = FACE_OUTER_BOUND ( 'NONE', #2108, .T. ) ;
#2049 = CARTESIAN_POINT ( 'NONE',  ( -5.584341313528829787, 39.74112841659670892, -140.1950701786490185 ) ) ;
#2050 = DIRECTION ( 'NONE',  ( 0.9944529286486341046, -0.1051825684329612265, -4.470295960598355531E-12 ) ) ;
#2051 = ORIENTED_EDGE ( 'NONE', *, *, #18360, .F. ) ;
#2052 = CARTESIAN_POINT ( 'NONE',  ( -32.50000000000000000, 14.00000000000000000, -144.0552959529999839 ) ) ;
#2053 = PLANE ( 'NONE',  #1485 ) ;
#2054 = ORIENTED_EDGE ( 'NONE', *, *, #12849, .F. ) ;
#2055 = VERTEX_POINT ( 'NONE', #4285 ) ;
#2056 = VECTOR ( 'NONE', #4505, 1000.000000000000000 ) ;
#2057 = EDGE_LOOP ( 'NONE', ( #5213, #12382, #8175, #20593 ) ) ;
#2058 = CARTESIAN_POINT ( 'NONE',  ( -46.00000000000000000, 37.00000000000000000, -149.5552959529999839 ) ) ;
#2059 = FACE_OUTER_BOUND ( 'NONE', #23094, .T. ) ;
#2060 = CARTESIAN_POINT ( 'NONE',  ( -22.33063748469999865, 35.38828378200000202, -140.2025093959999822 ) ) ;
#2061 = CARTESIAN_POINT ( 'NONE',  ( 7.643324914822369642, 35.76867410208022591, -141.8794674798148776 ) ) ;
#2062 = ORIENTED_EDGE ( 'NONE', *, *, #4013, .T. ) ;
#2063 = CARTESIAN_POINT ( 'NONE',  ( 19.75551406279999966, -31.14090339520000228, -144.5552959529999839 ) ) ;
#2064 = CARTESIAN_POINT ( 'NONE',  ( -18.36995524497817200, 33.45442790097475694, -146.2078216622589366 ) ) ;
#2065 = ADVANCED_FACE ( 'NONE', ( #16651 ), #2157, .F. ) ;
#2066 = CARTESIAN_POINT ( 'NONE',  ( 19.84954298759999958, -51.20423285660000090, -149.5552959529999839 ) ) ;
#2067 = DIRECTION ( 'NONE',  ( 1.000000000000000000, 0.000000000000000000, 0.000000000000000000 ) ) ;
#2068 = EDGE_CURVE ( 'NONE', #15863, #16606, #9880, .T. ) ;
#2069 = CARTESIAN_POINT ( 'NONE',  ( -32.50000000000000000, -36.00000000000000000, -137.0552959530000123 ) ) ;
#2070 = EDGE_CURVE ( 'NONE', #350, #12137, #20467, .T. ) ;
#2071 = CARTESIAN_POINT ( 'NONE',  ( -16.05159040817519056, 32.28373075711905926, -144.3107489965007062 ) ) ;
#2072 = VECTOR ( 'NONE', #16590, 1000.000000000000000 ) ;
#2073 = DIRECTION ( 'NONE',  ( -0.9792968044389154247, 0.2024296638729825848, -4.443945512649620152E-14 ) ) ;
#2074 = CARTESIAN_POINT ( 'NONE',  ( -3.500000000000000000, 44.50000000000000000, -150.0552959529999839 ) ) ;
#2075 = CARTESIAN_POINT ( 'NONE',  ( 3.999999999879999546, -3.000000000000000000, -135.2552959529999725 ) ) ;
#2076 = ORIENTED_EDGE ( 'NONE', *, *, #19643, .T. ) ;
#2077 = CARTESIAN_POINT ( 'NONE',  ( -7.010349701995939320, 37.05829245175783626, -148.1453878980124159 ) ) ;
#2078 = ORIENTED_EDGE ( 'NONE', *, *, #13262, .T. ) ;
#2079 = DIRECTION ( 'NONE',  ( 2.257749542879999954E-12, 0.000000000000000000, 1.000000000000000000 ) ) ;
#2080 = CARTESIAN_POINT ( 'NONE',  ( -46.00000000000000000, 26.50000000000000000, -149.0552959529999839 ) ) ;
#2081 = DIRECTION ( 'NONE',  ( 0.9980719161006958995, 0.06206811009758109871, -2.049912714059374948E-13 ) ) ;
#2082 = DIRECTION ( 'NONE',  ( 0.7071067811865473507, -0.7071067811865477948, 0.000000000000000000 ) ) ;
#2083 = CARTESIAN_POINT ( 'NONE',  ( -13.21931118294300056, 33.83281470423892046, -146.0365350582607959 ) ) ;
#2084 = CARTESIAN_POINT ( 'NONE',  ( 23.00000000000000000, 25.50000000000000000, -137.0552959530000123 ) ) ;
#2085 = CIRCLE ( 'NONE', #5489, 5.000000000000000000 ) ;
#2086 = PLANE ( 'NONE',  #2566 ) ;
#2087 = DIRECTION ( 'NONE',  ( -2.257144641399999941E-12, 0.000000000000000000, 1.000000000000000000 ) ) ;
#2088 = FACE_OUTER_BOUND ( 'NONE', #14523, .T. ) ;
#2089 = CARTESIAN_POINT ( 'NONE',  ( 3.298869075822184804, -4.420228454352442604, -136.0552959530074588 ) ) ;
#2090 = ORIENTED_EDGE ( 'NONE', *, *, #20324, .F. ) ;
#2091 = ADVANCED_FACE ( 'NONE', ( #22365 ), #7832, .F. ) ;
#2092 = UNCERTAINTY_MEASURE_WITH_UNIT (LENGTH_MEASURE( 1.000000000000000082E-05 ), #8479, 'distance_accuracy_value', 'NONE');
#2093 = ORIENTED_EDGE ( 'NONE', *, *, #19104, .T. ) ;
#2094 = ORIENTED_EDGE ( 'NONE', *, *, #16952, .F. ) ;
#2095 = LINE ( 'NONE', #22078, #1969 ) ;
#2096 = FACE_OUTER_BOUND ( 'NONE', #10710, .T. ) ;
#2097 = EDGE_LOOP ( 'NONE', ( #19263, #17599 ) ) ;
#2098 = CARTESIAN_POINT ( 'NONE',  ( 25.42371301062762257, 37.28076054105333270, -136.0552959530573673 ) ) ;
#2099 = EDGE_CURVE ( 'NONE', #14032, #4598, #22248, .T. ) ;
#2100 = DIRECTION ( 'NONE',  ( -2.257157423930000049E-12, 0.000000000000000000, -1.000000000000000000 ) ) ;
#2101 = LINE ( 'NONE', #14937, #8664 ) ;
#2102 = ORIENTED_EDGE ( 'NONE', *, *, #2124, .T. ) ;
#2103 = CARTESIAN_POINT ( 'NONE',  ( -20.31217984471907556, 37.68760996765858806, -140.7108956903404362 ) ) ;
#2104 = CARTESIAN_POINT ( 'NONE',  ( 8.811894473837091013, 38.46727147861445673, -142.0311810631515925 ) ) ;
#2105 = EDGE_CURVE ( 'NONE', #3167, #20530, #9376, .T. ) ;
#2106 = CARTESIAN_POINT ( 'NONE',  ( 10.00000000010000001, 37.00000000000000000, -138.5552959529999839 ) ) ;
#2107 = CARTESIAN_POINT ( 'NONE',  ( -23.90890255115609264, 36.92681688280359964, -147.8857207495020418 ) ) ;
#2108 = EDGE_LOOP ( 'NONE', ( #2629, #18054, #13739, #17573 ) ) ;
#2109 = EDGE_CURVE ( 'NONE', #16248, #22948, #20352, .T. ) ;
#2110 = CARTESIAN_POINT ( 'NONE',  ( 31.00000000000000000, 0.000000000000000000, -150.0552959529999839 ) ) ;
#2111 = VERTEX_POINT ( 'NONE', #11280 ) ;
#2112 = VECTOR ( 'NONE', #4682, 1000.000000000000000 ) ;
#2113 = CARTESIAN_POINT ( 'NONE',  ( 31.50000000000000000, -21.03620104879999886, -143.0552959529999839 ) ) ;
#2114 = VERTEX_POINT ( 'NONE', #2047 ) ;
#2115 = CARTESIAN_POINT ( 'NONE',  ( -26.09271177668468056, 41.23383702271284790, -143.6447300367354671 ) ) ;
#2116 = ORIENTED_EDGE ( 'NONE', *, *, #8857, .F. ) ;
#2117 = CARTESIAN_POINT ( 'NONE',  ( -22.25912899098128861, 34.38362928960210496, -140.2961181449622643 ) ) ;
#2118 = VERTEX_POINT ( 'NONE', #18682 ) ;
#2119 = CARTESIAN_POINT ( 'NONE',  ( -15.78524365307783306, -45.92191803000493877, -150.0552959529999839 ) ) ;
#2120 = VERTEX_POINT ( 'NONE', #11055 ) ;
#2121 =( LENGTH_UNIT ( ) NAMED_UNIT ( * ) SI_UNIT ( .MILLI., .METRE. ) );
#2122 = ORIENTED_EDGE ( 'NONE', *, *, #20027, .T. ) ;
#2123 = CARTESIAN_POINT ( 'NONE',  ( -27.48801997220000004, 39.21796412529999998, -147.0196846460000017 ) ) ;
#2124 = EDGE_CURVE ( 'NONE', #12686, #10612, #4164, .T. ) ;
#2125 = DIRECTION ( 'NONE',  ( 0.2229045288590935092, 0.9748402797454081004, -3.928002761761645078E-13 ) ) ;
#2126 = CARTESIAN_POINT ( 'NONE',  ( 13.24084097724026243, 23.82487805068920395, -150.0552959529999839 ) ) ;
#2127 = EDGE_CURVE ( 'NONE', #2852, #8980, #18335, .T. ) ;
#2128 = FACE_OUTER_BOUND ( 'NONE', #4122, .T. ) ;
#2129 = EDGE_CURVE ( 'NONE', #17215, #6070, #6064, .T. ) ;
#2130 = CARTESIAN_POINT ( 'NONE',  ( -10.24284460795958474, 35.44041190389086182, -140.1367555553470083 ) ) ;
#2131 = CARTESIAN_POINT ( 'NONE',  ( -8.325889011996979505, 41.57695941999546108, -143.5717776959861567 ) ) ;
#2132 = ORIENTED_EDGE ( 'NONE', *, *, #13601, .T. ) ;
#2133 = DIRECTION ( 'NONE',  ( 3.994014902821980611E-29, -1.000000000000000000, 4.148443855749775187E-27 ) ) ;
#2134 = AXIS2_PLACEMENT_3D ( 'NONE', #2956, #12223, #21048 ) ;
#2135 = VECTOR ( 'NONE', #11700, 1000.000000000000000 ) ;
#2136 = EDGE_CURVE ( 'NONE', #4706, #15489, #14753, .T. ) ;
#2137 = CARTESIAN_POINT ( 'NONE',  ( 8.842821505070592281, 35.53864366126496321, -146.0837389892870988 ) ) ;
#2138 = EDGE_CURVE ( 'NONE', #11594, #258, #11515, .T. ) ;
#2139 = ORIENTED_EDGE ( 'NONE', *, *, #3260, .T. ) ;
#2140 = DIRECTION ( 'NONE',  ( 2.255973186040000320E-12, 0.000000000000000000, 1.000000000000000000 ) ) ;
#2141 = ADVANCED_FACE ( 'NONE', ( #9615 ), #13193, .F. ) ;
#2142 = CARTESIAN_POINT ( 'NONE',  ( -11.69788097216356171, 37.87433970954386098, -139.6673822189363818 ) ) ;
#2143 = EDGE_CURVE ( 'NONE', #18702, #14446, #16539, .T. ) ;
#2144 = CARTESIAN_POINT ( 'NONE',  ( -17.53224077489999999, 39.64394931100000008, -140.2973660050000149 ) ) ;
#2145 = CARTESIAN_POINT ( 'NONE',  ( -30.02199999990000023, 40.03108891319999429, -145.8052959529999839 ) ) ;
#2146 = VERTEX_POINT ( 'NONE', #20243 ) ;
#2147 = CARTESIAN_POINT ( 'NONE',  ( -34.50000000000000000, -1.000000000000000000, -145.5552959529999839 ) ) ;
#2148 = CARTESIAN_POINT ( 'NONE',  ( 32.00000000000000000, -40.03620104880000241, -149.5552959529999839 ) ) ;
#2149 = VERTEX_POINT ( 'NONE', #3934 ) ;
#2150 = LINE ( 'NONE', #13074, #11375 ) ;
#2151 = DIRECTION ( 'NONE',  ( 0.000000000000000000, -1.000000000000000000, 0.000000000000000000 ) ) ;
#2152 = PLANE ( 'NONE',  #21239 ) ;
#2153 = VECTOR ( 'NONE', #16879, 1000.000000000000114 ) ;
#2154 = CARTESIAN_POINT ( 'NONE',  ( -21.06565549771221413, 41.62781742176859723, -143.5964485135013433 ) ) ;
#2155 = VERTEX_POINT ( 'NONE', #11170 ) ;
#2156 = CARTESIAN_POINT ( 'NONE',  ( -28.03429568402808059, 32.40695676816267934, -144.4586890253928004 ) ) ;
#2157 = PLANE ( 'NONE',  #9509 ) ;
#2158 = DIRECTION ( 'NONE',  ( -1.000000000000000000, 0.000000000000000000, 0.000000000000000000 ) ) ;
#2159 = CARTESIAN_POINT ( 'NONE',  ( 0.000000000000000000, 19.50000000000000000, -150.0552959529999839 ) ) ;
#2160 = DIRECTION ( 'NONE',  ( 2.257144641397284947E-12, -2.714590281723094849E-24, 1.000000000000000000 ) ) ;
#2161 = ORIENTED_EDGE ( 'NONE', *, *, #17520, .T. ) ;
#2162 = DIRECTION ( 'NONE',  ( 0.000000000000000000, -1.000000000000000000, 0.000000000000000000 ) ) ;
#2163 = CARTESIAN_POINT ( 'NONE',  ( -4.499999999949999996, 31.50000000000000000, -150.0552959529999839 ) ) ;
#2164 = VERTEX_POINT ( 'NONE', #16015 ) ;
#2165 =( BOUNDED_CURVE ( )  B_SPLINE_CURVE ( 5, ( #19574, #19333, #8956, #3044, #23260, #3161 ),
 .UNSPECIFIED., .F., .F. ) 
 B_SPLINE_CURVE_WITH_KNOTS ( ( 6, 6 ),
 ( 1.570796326630344186, 3.141592653590000062 ),
 .UNSPECIFIED. ) 
 CURVE ( )  GEOMETRIC_REPRESENTATION_ITEM ( )  RATIONAL_B_SPLINE_CURVE ( ( 0.2500000000000000555, 0.2499999999790353811, 0.2999999999685530883, 0.3999999999580707288, 0.5999999999580707399, 1.000000000000000000 ) ) 
 REPRESENTATION_ITEM ( '' )  );
#2166 = EDGE_CURVE ( 'NONE', #14118, #10634, #8177, .T. ) ;
#2167 = AXIS2_PLACEMENT_3D ( 'NONE', #6419, #4646, #10091 ) ;
#2168 = EDGE_LOOP ( 'NONE', ( #4075, #9774, #2218, #5035 ) ) ;
#2169 = CARTESIAN_POINT ( 'NONE',  ( -23.22224815339999893, 34.57381638260000045, -140.7548632179999970 ) ) ;
#2170 = CARTESIAN_POINT ( 'NONE',  ( 31.96891336220000213, -40.94938100119999547, -149.5552959529999839 ) ) ;
#2171 = LINE ( 'NONE', #18112, #10515 ) ;
#2172 = CARTESIAN_POINT ( 'NONE',  ( 7.966339544912719894, 35.59716178443439105, -141.9858703028249067 ) ) ;
#2173 = ORIENTED_EDGE ( 'NONE', *, *, #18480, .F. ) ;
#2174 = LINE ( 'NONE', #9984, #7127 ) ;
#2175 = CARTESIAN_POINT ( 'NONE',  ( -20.13043194029999938, 34.25277599949999541, -140.5881547479999938 ) ) ;
#2176 = DIRECTION ( 'NONE',  ( -1.449507180940000069E-12, -1.705302565810000055E-12, 1.000000000000000000 ) ) ;
#2177 = LINE ( 'NONE', #2525, #1223 ) ;
#2178 = CARTESIAN_POINT ( 'NONE',  ( -24.21201708719999957, 40.99356323119999956, -143.6328343570000072 ) ) ;
#2179 = CARTESIAN_POINT ( 'NONE',  ( -14.84561440076392458, 36.91926241633398575, -147.9647079511927927 ) ) ;
#2180 = CIRCLE ( 'NONE', #20413, 2.999999999999999112 ) ;
#2181 = AXIS2_PLACEMENT_3D ( 'NONE', #3165, #15655, #10503 ) ;
#2182 = PLANE ( 'NONE',  #20224 ) ;
#2183 = LINE ( 'NONE', #515, #19455 ) ;
#2184 = CARTESIAN_POINT ( 'NONE',  ( -13.86630785130000021, -51.00000000000000000, -137.0552959530000123 ) ) ;
#2185 = ORIENTED_EDGE ( 'NONE', *, *, #5828, .F. ) ;
#2186 = CARTESIAN_POINT ( 'NONE',  ( -5.941327522415615903, 39.27619043351264594, -140.7701191936981218 ) ) ;
#2187 = ORIENTED_EDGE ( 'NONE', *, *, #11432, .F. ) ;
#2188 = FACE_OUTER_BOUND ( 'NONE', #13050, .T. ) ;
#2189 = EDGE_CURVE ( 'NONE', #19467, #19419, #6288, .T. ) ;
#2190 = DIRECTION ( 'NONE',  ( 0.3989061605089001539, 0.7301928289268172501, 0.5547001962248612195 ) ) ;
#2191 = EDGE_CURVE ( 'NONE', #4452, #11004, #2968, .T. ) ;
#2192 = CARTESIAN_POINT ( 'NONE',  ( -24.32282749495824703, 36.01414085272633514, -148.6131980735590901 ) ) ;
#2193 = ORIENTED_EDGE ( 'NONE', *, *, #5142, .F. ) ;
#2194 = CARTESIAN_POINT ( 'NONE',  ( -11.85909339608079094, 36.92087135288664967, -147.9691652862316857 ) ) ;
#2195 = VECTOR ( 'NONE', #14891, 1000.000000000000000 ) ;
#2196 = CARTESIAN_POINT ( 'NONE',  ( 3.611688725869999975E-11, 25.50000000000000000, -136.0552959530000123 ) ) ;
#2197 = PRESENTATION_LAYER_ASSIGNMENT (  '', '', ( #19668 ) ) ;
#2198 = CARTESIAN_POINT ( 'NONE',  ( -21.35824191589999899, -32.00000000000000000, -144.8157682190000060 ) ) ;
#2199 = FACE_OUTER_BOUND ( 'NONE', #7681, .T. ) ;
#2200 = DIRECTION ( 'NONE',  ( -1.000000000000000000, 5.094701932209999624E-24, 0.000000000000000000 ) ) ;
#2201 = CARTESIAN_POINT ( 'NONE',  ( 7.683200060759999950, -19.50000000000000000, -148.5552959529999839 ) ) ;
#2202 = APPLICATION_CONTEXT ( 'automotive_design' ) ;
#2203 = EDGE_LOOP ( 'NONE', ( #7447, #5726, #22489, #13678 ) ) ;
#2204 =( BOUNDED_CURVE ( )  B_SPLINE_CURVE ( 5, ( #23313, #2029, #1559, #7362, #1676, #14622, #19626, #7006, #14156, #5465, #12823, #16294 ),
 .UNSPECIFIED., .F., .F. ) 
 B_SPLINE_CURVE_WITH_KNOTS ( ( 6, 3, 3, 6 ),
 ( 0.000000000000000000, 4.066159495680000013, 8.252146144990000209, 12.56898909049999880 ),
 .UNSPECIFIED. ) 
 CURVE ( )  GEOMETRIC_REPRESENTATION_ITEM ( )  RATIONAL_B_SPLINE_CURVE ( ( 0.2500000000000000000, 0.2500000000000000000, 0.2500000000000000000, 0.2500000000000000000, 0.2500000000000000000, 0.2500000000000000000, 0.2500000000000000000, 0.2500000000000000000, 0.2500000000000000000, 0.2500000000000000000, 0.2500000000000000000, 0.2500000000000000000 ) ) 
 REPRESENTATION_ITEM ( '' )  );
#2205 = LINE ( 'NONE', #3981, #8691 ) ;
#2206 = ORIENTED_EDGE ( 'NONE', *, *, #20348, .T. ) ;
#2207 =( LENGTH_UNIT ( ) NAMED_UNIT ( * ) SI_UNIT ( .MILLI., .METRE. ) );
#2208 = ORIENTED_EDGE ( 'NONE', *, *, #21074, .T. ) ;
#2209 = CARTESIAN_POINT ( 'NONE',  ( -13.80638726114959169, 32.41177233165633709, -143.7882581758906611 ) ) ;
#2210 = LINE ( 'NONE', #15041, #12594 ) ;
#2211 = CYLINDRICAL_SURFACE ( 'NONE', #10765, 1.499999999999999556 ) ;
#2212 = AXIS2_PLACEMENT_3D ( 'NONE', #7400, #20372, #18578 ) ;
#2213 = VERTEX_POINT ( 'NONE', #1200 ) ;
#2214 = LINE ( 'NONE', #9435, #17096 ) ;
#2215 = LINE ( 'NONE', #13488, #6466 ) ;
#2216 = VECTOR ( 'NONE', #13785, 1000.000000000000000 ) ;
#2217 = DIRECTION ( 'NONE',  ( -1.000000000000000000, 5.094701932209999624E-24, 0.000000000000000000 ) ) ;
#2218 = ORIENTED_EDGE ( 'NONE', *, *, #14621, .F. ) ;
#2219 = CARTESIAN_POINT ( 'NONE',  ( -21.50444101780000139, 40.78041997809999941, -146.2395182369999986 ) ) ;
#2220 = EDGE_CURVE ( 'NONE', #7796, #10437, #12426, .T. ) ;
#2221 = CARTESIAN_POINT ( 'NONE',  ( 9.809232433496585912, 37.73246533773845357, -141.6649243764299797 ) ) ;
#2222 = EDGE_CURVE ( 'NONE', #13428, #6792, #22485, .T. ) ;
#2223 = LINE ( 'NONE', #4348, #16177 ) ;
#2224 = FACE_OUTER_BOUND ( 'NONE', #14982, .T. ) ;
#2225 = ORIENTED_EDGE ( 'NONE', *, *, #4013, .F. ) ;
#2226 = CIRCLE ( 'NONE', #5252, 1.500000000000001332 ) ;
#2227 = LINE ( 'NONE', #7560, #3466 ) ;
#2228 = STYLED_ITEM ( 'NONE', ( #4378 ), #20016 ) ;
#2229 = ORIENTED_EDGE ( 'NONE', *, *, #7906, .T. ) ;
#2230 = CARTESIAN_POINT ( 'NONE',  ( 4.750000000000000000, -47.00000000000000000, -150.0552959529999839 ) ) ;
#2231 = ORIENTED_EDGE ( 'NONE', *, *, #16925, .F. ) ;
#2232 = CARTESIAN_POINT ( 'NONE',  ( -26.20001943430085589, 40.80945677298473129, -144.5049606645992242 ) ) ;
#2233 = EDGE_LOOP ( 'NONE', ( #616, #16482, #10341, #10938 ) ) ;
#2234 = CARTESIAN_POINT ( 'NONE',  ( -22.43192306081355269, 32.22142746413794612, -144.5072135593746623 ) ) ;
#2235 = ORIENTED_EDGE ( 'NONE', *, *, #2191, .T. ) ;
#2236 = DIRECTION ( 'NONE',  ( 1.000000000000000000, 0.000000000000000000, 0.000000000000000000 ) ) ;
#2237 = VERTEX_POINT ( 'NONE', #20696 ) ;
#2238 = ADVANCED_FACE ( 'NONE', ( #11990 ), #3397, .T. ) ;
#2239 = EDGE_LOOP ( 'NONE', ( #17435, #8425, #9225, #4011, #20545 ) ) ;
#2240 = CARTESIAN_POINT ( 'NONE',  ( -29.29455083643873436, 36.96746664034499474, -139.4767999531160569 ) ) ;
#2241 = CARTESIAN_POINT ( 'NONE',  ( 13.13369214870000157, 51.00000000000000000, -136.0552959530000123 ) ) ;
#2242 = LINE ( 'NONE', #13281, #9188 ) ;
#2243 = CARTESIAN_POINT ( 'NONE',  ( -2.599999999940000084, 37.00000000000000000, -144.0552959529999839 ) ) ;
#2244 = CARTESIAN_POINT ( 'NONE',  ( -6.938784185764153456, 37.04974994750939032, -148.5388410751212120 ) ) ;
#2245 = VECTOR ( 'NONE', #18530, 1000.000000000000000 ) ;
#2246 = CARTESIAN_POINT ( 'NONE',  ( -4.499999999939999995, 39.19395640469999620, -145.2538597989999971 ) ) ;
#2247 = EDGE_LOOP ( 'NONE', ( #14580, #18347, #13625 ) ) ;
#2248 = VECTOR ( 'NONE', #22620, 1000.000000000000000 ) ;
#2249 = CARTESIAN_POINT ( 'NONE',  ( 13.68320006080000084, -21.50000000000000000, -138.5552959529999839 ) ) ;
#2250 = EDGE_CURVE ( 'NONE', #7971, #2516, #14233, .T. ) ;
#2251 = CIRCLE ( 'NONE', #10589, 1.000000000000000888 ) ;
#2252 = CARTESIAN_POINT ( 'NONE',  ( 12.68320006080000084, -24.50000000000000000, -148.5552959529999839 ) ) ;
#2253 = VECTOR ( 'NONE', #14511, 1000.000000000000227 ) ;
#2254 = ORIENTED_EDGE ( 'NONE', *, *, #12139, .F. ) ;
#2255 = CARTESIAN_POINT ( 'NONE',  ( -7.499999999959999997, 45.50000000000000000, -136.0552959530000123 ) ) ;
#2256 = CARTESIAN_POINT ( 'NONE',  ( -12.47185022218380723, 37.93970414752843823, -148.6532233943605661 ) ) ;
#2257 = EDGE_CURVE ( 'NONE', #6729, #16039, #20814, .T. ) ;
#2258 = CARTESIAN_POINT ( 'NONE',  ( -4.499999999939999995, 37.00000000000000000, -144.0552959529999839 ) ) ;
#2259 = CARTESIAN_POINT ( 'NONE',  ( -29.13556667879501560, 41.19822702818812132, -144.4115419828412996 ) ) ;
#2260 = ORIENTED_EDGE ( 'NONE', *, *, #9977, .T. ) ;
#2261 = CARTESIAN_POINT ( 'NONE',  ( 24.75935218339999722, -28.32938697159999819, -147.5552959529999839 ) ) ;
#2262 = PLANE ( 'NONE',  #18458 ) ;
#2263 = AXIS2_PLACEMENT_3D ( 'NONE', #16207, #18662, #23458 ) ;
#2264 = EDGE_LOOP ( 'NONE', ( #18770, #22845, #17331, #9934 ) ) ;
#2265 = LINE ( 'NONE', #7714, #17477 ) ;
#2266 = CARTESIAN_POINT ( 'NONE',  ( -28.50747929780000334, 33.37084171139999711, -143.6371486329999811 ) ) ;
#2267 = ORIENTED_EDGE ( 'NONE', *, *, #9759, .T. ) ;
#2268 = CARTESIAN_POINT ( 'NONE',  ( 22.50000000000000000, 36.50000000000000000, -151.0552959529999839 ) ) ;
#2269 = AXIS2_PLACEMENT_3D ( 'NONE', #15309, #15537, #19221 ) ;
#2270 = CARTESIAN_POINT ( 'NONE',  ( -20.43858045619872144, 40.80995393214885780, -146.3951808076467955 ) ) ;
#2271 = VERTEX_POINT ( 'NONE', #11746 ) ;
#2272 = FILL_AREA_STYLE_COLOUR ( '', #5063 ) ;
#2273 = DIRECTION ( 'NONE',  ( 1.000000000000000000, 0.000000000000000000, 0.000000000000000000 ) ) ;
#2274 = AXIS2_PLACEMENT_3D ( 'NONE', #1100, #20972, #1227 ) ;
#2275 = EDGE_CURVE ( 'NONE', #13585, #13529, #13797, .T. ) ;
#2276 = DIRECTION ( 'NONE',  ( 0.07970438983373200059, 0.9968185442904001770, -8.242295734823311485E-13 ) ) ;
#2277 = VERTEX_POINT ( 'NONE', #13542 ) ;
#2278 = AXIS2_PLACEMENT_3D ( 'NONE', #12325, #19839, #14245 ) ;
#2279 = DIRECTION ( 'NONE',  ( -1.211690350419999855E-27, -2.765629237170000203E-27, 1.000000000000000000 ) ) ;
#2280 = EDGE_CURVE ( 'NONE', #4867, #17914, #19704, .T. ) ;
#2281 = FACE_OUTER_BOUND ( 'NONE', #7195, .T. ) ;
#2282 = CARTESIAN_POINT ( 'NONE',  ( -32.50000000000000000, 48.00000000000000000, -139.5552959529999839 ) ) ;
#2283 = EDGE_CURVE ( 'NONE', #2271, #4317, #10201, .T. ) ;
#2284 = VERTEX_POINT ( 'NONE', #19026 ) ;
#2285 = DIRECTION ( 'NONE',  ( 1.000000000000000000, -1.190078432789999897E-50, -2.257144641399999941E-12 ) ) ;
#2286 = ADVANCED_FACE ( 'NONE', ( #22597 ), #4744, .F. ) ;
#2287 = CARTESIAN_POINT ( 'NONE',  ( 8.500000000050000892, 37.00000000000000000, -149.5552959529999839 ) ) ;
#2288 = ORIENTED_EDGE ( 'NONE', *, *, #13914, .F. ) ;
#2289 = AXIS2_PLACEMENT_3D ( 'NONE', #8985, #19840, #1532 ) ;
#2290 = VECTOR ( 'NONE', #22504, 1000.000000000000227 ) ;
#2291 = EDGE_LOOP ( 'NONE', ( #6808, #15232, #13159, #14299, #8994, #19423, #18000, #15179 ) ) ;
#2292 = AXIS2_PLACEMENT_3D ( 'NONE', #17739, #21989, #19535 ) ;
#2293 = AXIS2_PLACEMENT_3D ( 'NONE', #20911, #22681, #4836 ) ;
#2294 = DIRECTION ( 'NONE',  ( -2.507771768019999718E-12, -1.592654864069999939E-17, 1.000000000000000000 ) ) ;
#2295 = CARTESIAN_POINT ( 'NONE',  ( 32.50000000000000000, 20.96379895120000114, -137.0552959530000123 ) ) ;
#2296 = LINE ( 'NONE', #9166, #673 ) ;
#2297 = CARTESIAN_POINT ( 'NONE',  ( 7.651143207404245139, 35.76327648575674090, -141.8825763915462517 ) ) ;
#2298 = ORIENTED_EDGE ( 'NONE', *, *, #620, .T. ) ;
#2299 =( NAMED_UNIT ( * ) PLANE_ANGLE_UNIT ( ) SI_UNIT ( $, .RADIAN. ) );
#2300 = DIRECTION ( 'NONE',  ( 0.000000000000000000, 0.000000000000000000, 1.000000000000000000 ) ) ;
#2301 = DIRECTION ( 'NONE',  ( -1.457985068979999943E-12, 1.723073263340000007E-12, 1.000000000000000000 ) ) ;
#2302 = PLANE ( 'NONE',  #10309 ) ;
#2303 = CARTESIAN_POINT ( 'NONE',  ( -24.99548980007219612, 37.05651868163715790, -148.5304149358840675 ) ) ;
#2304 = CARTESIAN_POINT ( 'NONE',  ( -15.37195868313349045, 34.69747584690560416, -146.9441783042220493 ) ) ;
#2305 = EDGE_CURVE ( 'NONE', #10668, #11605, #4633, .T. ) ;
#2306 = ADVANCED_FACE ( 'NONE', ( #4389 ), #11628, .F. ) ;
#2307 = FACE_OUTER_BOUND ( 'NONE', #5624, .T. ) ;
#2308 = CARTESIAN_POINT ( 'NONE',  ( -30.49999999990000177, 46.25000000000000000, -147.5552959529999839 ) ) ;
#2309 = LINE ( 'NONE', #7980, #13067 ) ;
#2310 = AXIS2_PLACEMENT_3D ( 'NONE', #785, #6000, #16948 ) ;
#2311 = VECTOR ( 'NONE', #4811, 1000.000000000000000 ) ;
#2312 = ORIENTED_EDGE ( 'NONE', *, *, #13738, .T. ) ;
#2313 = AXIS2_PLACEMENT_3D ( 'NONE', #12312, #21258, #12198 ) ;
#2314 = CARTESIAN_POINT ( 'NONE',  ( -6.194210391756115541, 38.39815610428787807, -147.2141978122577939 ) ) ;
#2315 = DIRECTION ( 'NONE',  ( -0.9919007982877544594, 0.1270149847699686418, 4.766005912188822159E-14 ) ) ;
#2316 = ORIENTED_EDGE ( 'NONE', *, *, #12600, .T. ) ;
#2317 = FACE_OUTER_BOUND ( 'NONE', #19183, .T. ) ;
#2318 = DIRECTION ( 'NONE',  ( -0.07970438983373200059, -0.9968185442904001770, 8.268133652483321323E-13 ) ) ;
#2319 = ORIENTED_EDGE ( 'NONE', *, *, #6179, .T. ) ;
#2320 = FACE_OUTER_BOUND ( 'NONE', #1264, .T. ) ;
#2321 = PLANE ( 'NONE',  #20385 ) ;
#2322 = LINE ( 'NONE', #5982, #8614 ) ;
#2323 = CARTESIAN_POINT ( 'NONE',  ( 19.04211518580000018, -51.50000000000000000, -150.0552959529999839 ) ) ;
#2324 = AXIS2_PLACEMENT_3D ( 'NONE', #13079, #15231, #7950 ) ;
#2325 = FACE_OUTER_BOUND ( 'NONE', #5206, .T. ) ;
#2326 = VECTOR ( 'NONE', #19118, 1000.000000000000000 ) ;
#2327 = LINE ( 'NONE', #4092, #2595 ) ;
#2328 = ORIENTED_EDGE ( 'NONE', *, *, #3849, .F. ) ;
#2329 = LINE ( 'NONE', #9424, #742 ) ;
#2330 = VERTEX_POINT ( 'NONE', #2615 ) ;
#2331 = SURFACE_STYLE_FILL_AREA ( #895 ) ;
#2332 = ADVANCED_FACE ( 'NONE', ( #9846 ), #19143, .F. ) ;
#2333 = ORIENTED_EDGE ( 'NONE', *, *, #4922, .F. ) ;
#2334 = FACE_OUTER_BOUND ( 'NONE', #22804, .T. ) ;
#2335 = CARTESIAN_POINT ( 'NONE',  ( 2.499999999879999990, -3.500000000000000000, -135.4552959529999896 ) ) ;
#2336 = DIRECTION ( 'NONE',  ( -1.000000000000000000, 0.000000000000000000, 2.257453483404482811E-12 ) ) ;
#2337 = VERTEX_POINT ( 'NONE', #2846 ) ;
#2338 = CARTESIAN_POINT ( 'NONE',  ( 4.999999999879999990, -3.500000000000000000, -132.9059375850000038 ) ) ;
#2339 = DIRECTION ( 'NONE',  ( 1.000000000000000000, 2.602084704497994558E-17, -1.701177080612860179E-20 ) ) ;
#2340 = AXIS2_PLACEMENT_3D ( 'NONE', #10063, #10187, #20801 ) ;
#2341 = ORIENTED_EDGE ( 'NONE', *, *, #15619, .F. ) ;
#2342 = PRESENTATION_LAYER_ASSIGNMENT (  '', '', ( #11802 ) ) ;
#2343 = CARTESIAN_POINT ( 'NONE',  ( 14.00000000000000000, 20.50000000000000000, -136.0552959530000123 ) ) ;
#2344 = CARTESIAN_POINT ( 'NONE',  ( 9.593201079431377565, 38.02725237339706155, -141.7760678466342767 ) ) ;
#2345 = DIRECTION ( 'NONE',  ( 1.000000000000000000, 0.000000000000000000, 0.000000000000000000 ) ) ;
#2346 = DIRECTION ( 'NONE',  ( 0.000000000000000000, -1.000000000000000000, 0.000000000000000000 ) ) ;
#2347 = ORIENTED_EDGE ( 'NONE', *, *, #4982, .F. ) ;
#2348 =( BOUNDED_SURFACE ( )  B_SPLINE_SURFACE ( 5, 5, ( 
 ( #9323, #22086, #13382, #12910, #20531, #3887 ),
 ( #7551, #18392, #2103, #22308, #4105, #14827 ),
 ( #550, #22199, #9567, #658, #20193, #4343 ),
 ( #8013, #9440, #16596, #310, #5774, #20412 ),
 ( #4232, #11577, #6125, #2564, #11467, #17065 ),
 ( #787, #15295, #7783, #22551, #13033, #15050 ),
 ( #6003, #9675, #20304, #3994, #11227, #16951 ),
 ( #7891, #15171, #22430, #18500, #5886, #2219 ),
 ( #16717, #432, #7670, #14939, #13741, #3156 ),
 ( #15520, #12057, #21005, #10386, #6592, #22781 ),
 ( #22908, #2799, #19458, #6480, #4697, #20765 ),
 ( #13611, #19328, #17662, #4935, #9913, #8490 ) ),
 .UNSPECIFIED., .F., .F., .F. ) 
 B_SPLINE_SURFACE_WITH_KNOTS ( ( 6, 3, 3, 6 ),
 ( 6, 6 ),
 ( 0.000000000000000000, 4.390059406679999832, 8.746277600790000051, 13.07048654049999925 ),
 ( 1.570796326526080033, 3.141592653590000062 ),
 .UNSPECIFIED. ) 
 GEOMETRIC_REPRESENTATION_ITEM ( )  RATIONAL_B_SPLINE_SURFACE ( (
 ( 0.2500000000000000000, 0.2499999999657600003, 0.2999999999486395175, 0.3999999999315194676, 0.5999999999315199783, 1.000000000000000000),
 ( 0.2500000000000000000, 0.2499999999657600003, 0.2999999999486395175, 0.3999999999315194676, 0.5999999999315199783, 1.000000000000000000),
 ( 0.2500000000000000000, 0.2499999999657600003, 0.2999999999486395175, 0.3999999999315194676, 0.5999999999315199783, 1.000000000000000000),
 ( 0.2500000000000000000, 0.2499999999657600003, 0.2999999999486395175, 0.3999999999315194676, 0.5999999999315199783, 1.000000000000000000),
 ( 0.2500000000000000000, 0.2499999999657600003, 0.2999999999486395175, 0.3999999999315194676, 0.5999999999315199783, 1.000000000000000000),
 ( 0.2500000000000000000, 0.2499999999657600003, 0.2999999999486395175, 0.3999999999315194676, 0.5999999999315199783, 1.000000000000000000),
 ( 0.2500000000000000000, 0.2499999999657600003, 0.2999999999486395175, 0.3999999999315194676, 0.5999999999315199783, 1.000000000000000000),
 ( 0.2500000000000000000, 0.2499999999657600003, 0.2999999999486395175, 0.3999999999315194676, 0.5999999999315199783, 1.000000000000000000),
 ( 0.2500000000000000000, 0.2499999999657600003, 0.2999999999486395175, 0.3999999999315194676, 0.5999999999315199783, 1.000000000000000000),
 ( 0.2500000000000000000, 0.2499999999657600003, 0.2999999999486395175, 0.3999999999315194676, 0.5999999999315199783, 1.000000000000000000),
 ( 0.2500000000000000000, 0.2499999999657600003, 0.2999999999486395175, 0.3999999999315194676, 0.5999999999315199783, 1.000000000000000000),
 ( 0.2500000000000000000, 0.2499999999657600003, 0.2999999999486395175, 0.3999999999315194676, 0.5999999999315199783, 1.000000000000000000) ) ) 
 REPRESENTATION_ITEM ( '' )  SURFACE ( )  );
#2349 = DIRECTION ( 'NONE',  ( 0.000000000000000000, 0.000000000000000000, -1.000000000000000000 ) ) ;
#2350 = ORIENTED_EDGE ( 'NONE', *, *, #15505, .T. ) ;
#2351 = CARTESIAN_POINT ( 'NONE',  ( 8.698929461718192258, -47.52072668388614574, -150.0552959530000123 ) ) ;
#2352 = CIRCLE ( 'NONE', #11816, 5.999999999999998224 ) ;
#2353 = VECTOR ( 'NONE', #1166, 1000.000000000000114 ) ;
#2354 = ADVANCED_FACE ( 'NONE', ( #17353 ), #1068, .T. ) ;
#2355 = EDGE_LOOP ( 'NONE', ( #21561, #2696, #15045, #934, #13188, #21639, #9708, #5880 ) ) ;
#2356 = CARTESIAN_POINT ( 'NONE',  ( -25.46206384012266710, 37.06683745572687627, -140.4480127386052004 ) ) ;
#2357 = ORIENTED_EDGE ( 'NONE', *, *, #18288, .F. ) ;
#2358 = EDGE_CURVE ( 'NONE', #8373, #12827, #5767, .T. ) ;
#2359 = CARTESIAN_POINT ( 'NONE',  ( -22.33063748467256104, 35.38828378206188319, -140.2025093961515836 ) ) ;
#2360 = VERTEX_POINT ( 'NONE', #7431 ) ;
#2361 = DIRECTION ( 'NONE',  ( -0.6459422414661292189, 0.7633862853691524286, 1.457985068980292769E-12 ) ) ;
#2362 = EDGE_CURVE ( 'NONE', #14060, #11337, #12904, .T. ) ;
#2363 = ORIENTED_EDGE ( 'NONE', *, *, #956, .F. ) ;
#2364 = DIRECTION ( 'NONE',  ( 1.000000000000000000, 0.000000000000000000, 0.000000000000000000 ) ) ;
#2365 = ORIENTED_EDGE ( 'NONE', *, *, #6046, .F. ) ;
#2366 = CARTESIAN_POINT ( 'NONE',  ( 18.95053822279999878, 51.50000000000000000, -149.5552959529999839 ) ) ;
#2367 = DIRECTION ( 'NONE',  ( 0.7633862853691524286, -0.6459422414661293299, 0.000000000000000000 ) ) ;
#2368 = LINE ( 'NONE', #22110, #18943 ) ;
#2369 = CARTESIAN_POINT ( 'NONE',  ( -7.816799939239999162, 0.9999999999989999111, -148.5552959529999839 ) ) ;
#2370 = CARTESIAN_POINT ( 'NONE',  ( -7.529689113779999943, 37.05876528330000497, -139.9906690790000141 ) ) ;
#2371 = VERTEX_POINT ( 'NONE', #21854 ) ;
#2372 = CARTESIAN_POINT ( 'NONE',  ( 13.13369214859999978, 50.50000000000000000, -142.8052959529999839 ) ) ;
#2373 = AXIS2_PLACEMENT_3D ( 'NONE', #5090, #12334, #19611 ) ;
#2374 = AXIS2_PLACEMENT_3D ( 'NONE', #3874, #20644, #11111 ) ;
#2375 = AXIS2_PLACEMENT_3D ( 'NONE', #5266, #23475, #273 ) ;
#2376 = CARTESIAN_POINT ( 'NONE',  ( -30.49999999990000177, 26.50000000000000000, -139.8052959529999839 ) ) ;
#2377 = FACE_OUTER_BOUND ( 'NONE', #6841, .T. ) ;
#2378 = ORIENTED_EDGE ( 'NONE', *, *, #7878, .F. ) ;
#2379 = CARTESIAN_POINT ( 'NONE',  ( -10.76224745929999926, 37.97907322949999553, -139.7231730900000173 ) ) ;
#2380 = CARTESIAN_POINT ( 'NONE',  ( -17.39663711204255492, 40.51543712901364103, -146.0950904568249484 ) ) ;
#2381 = CARTESIAN_POINT ( 'NONE',  ( -29.19363900808597734, 40.77773483849115621, -144.3769002367588428 ) ) ;
#2382 = ORIENTED_EDGE ( 'NONE', *, *, #1560, .F. ) ;
#2383 = CARTESIAN_POINT ( 'NONE',  ( 13.68320006080000084, -19.50000000000000000, -138.5552959529999839 ) ) ;
#2384 = CYLINDRICAL_SURFACE ( 'NONE', #1761, 2.500000000000002220 ) ;
#2385 = ORIENTED_EDGE ( 'NONE', *, *, #4992, .T. ) ;
#2386 = CARTESIAN_POINT ( 'NONE',  ( -33.50000000000000000, 28.00000000000000000, -141.5552959529999839 ) ) ;
#2387 = CARTESIAN_POINT ( 'NONE',  ( 22.33963087269999903, -30.94765732060000119, -146.5552959529999839 ) ) ;
#2388 = VERTEX_POINT ( 'NONE', #3877 ) ;
#2389 = CARTESIAN_POINT ( 'NONE',  ( -5.246523349696126104, 45.51000832343219571, -150.0552959530000123 ) ) ;
#2390 = CARTESIAN_POINT ( 'NONE',  ( -21.80913741070000000, 38.74859698539999897, -147.9243209519999880 ) ) ;
#2391 = EDGE_CURVE ( 'NONE', #10437, #23049, #300, .T. ) ;
#2392 = ORIENTED_EDGE ( 'NONE', *, *, #826, .F. ) ;
#2393 = VECTOR ( 'NONE', #601, 1000.000000000000000 ) ;
#2394 = CARTESIAN_POINT ( 'NONE',  ( -27.97684248819999908, 35.51254237909999745, -147.4365014880000047 ) ) ;
#2395 = CARTESIAN_POINT ( 'NONE',  ( -9.157754307290000284, -15.75963164970000108, -147.5552959529999839 ) ) ;
#2396 = VERTEX_POINT ( 'NONE', #21617 ) ;
#2397 = CARTESIAN_POINT ( 'NONE',  ( 21.79964646190000011, -30.87346604779999737, -145.5552959529999839 ) ) ;
#2398 = LINE ( 'NONE', #11172, #14153 ) ;
#2399 = CARTESIAN_POINT ( 'NONE',  ( -35.33948162989999986, 11.17737245070000185, -144.5552959529999839 ) ) ;
#2400 = ORIENTED_EDGE ( 'NONE', *, *, #3159, .T. ) ;
#2401 = LINE ( 'NONE', #2511, #22001 ) ;
#2402 = ADVANCED_FACE ( 'NONE', ( #21961 ), #2211, .F. ) ;
#2403 = CARTESIAN_POINT ( 'NONE',  ( -32.50000000000000000, -1.000000000000000000, -151.0552959529999839 ) ) ;
#2404 = ORIENTED_EDGE ( 'NONE', *, *, #22120, .F. ) ;
#2405 = COLOUR_RGB ( '', 0.09019608, 0.27058824, 0.51372549) ;
#2406 = ORIENTED_EDGE ( 'NONE', *, *, #4979, .T. ) ;
#2407 = AXIS2_PLACEMENT_3D ( 'NONE', #1642, #3177, #3645 ) ;
#2408 = CARTESIAN_POINT ( 'NONE',  ( 5.257430384941513601, -2.190056847782472005, -136.0552959530118642 ) ) ;
#2409 = EDGE_CURVE ( 'NONE', #22806, #17118, #7206, .T. ) ;
#2410 = FACE_OUTER_BOUND ( 'NONE', #1741, .T. ) ;
#2411 = CARTESIAN_POINT ( 'NONE',  ( -18.85469010170000459, 37.03971195569999963, -148.4264296979999926 ) ) ;
#2412 = CARTESIAN_POINT ( 'NONE',  ( 7.898597776409067350, 35.62582981816382954, -141.9668508539811285 ) ) ;
#2413 = ORIENTED_EDGE ( 'NONE', *, *, #23486, .T. ) ;
#2414 = DIRECTION ( 'NONE',  ( 1.000000000000000000, 0.000000000000000000, -2.257453483404485639E-12 ) ) ;
#2415 = CARTESIAN_POINT ( 'NONE',  ( -8.238646733050000392, 41.24792906369999912, -143.6196368420000056 ) ) ;
#2416 = EDGE_CURVE ( 'NONE', #7470, #5894, #5301, .T. ) ;
#2417 = CARTESIAN_POINT ( 'NONE',  ( -32.50000000000000000, -43.00000000000000000, -149.5552959529999839 ) ) ;
#2418 = CARTESIAN_POINT ( 'NONE',  ( -9.801780388952463952, 37.03339632390886038, -147.4803110668171939 ) ) ;
#2419 = EDGE_CURVE ( 'NONE', #19198, #4115, #5647, .T. ) ;
#2420 = CARTESIAN_POINT ( 'NONE',  ( -23.68820627306414295, 41.09826978516893092, -146.5293788421483043 ) ) ;
#2421 = DIRECTION ( 'NONE',  ( -1.000000000000000000, 0.000000000000000000, 2.273736754430000208E-12 ) ) ;
#2422 = CARTESIAN_POINT ( 'NONE',  ( -17.13033207850000039, 36.08498863180000171, -139.6042211940000186 ) ) ;
#2423 = DIRECTION ( 'NONE',  ( 0.000000000000000000, 1.000000000000000000, 0.000000000000000000 ) ) ;
#2424 = CARTESIAN_POINT ( 'NONE',  ( -15.00000000000000000, -41.50000000000000000, -137.0552959530000123 ) ) ;
#2425 = STYLED_ITEM ( 'NONE', ( #4984 ), #18345 ) ;
#2426 = LINE ( 'NONE', #16805, #21069 ) ;
#2427 = EDGE_LOOP ( 'NONE', ( #7115, #6147, #20649, #23007 ) ) ;
#2428 = CARTESIAN_POINT ( 'NONE',  ( -4.933950775581154247, 38.47208611112608878, -140.7832461089165292 ) ) ;
#2429 = FACE_BOUND ( 'NONE', #16832, .T. ) ;
#2430 = ADVANCED_FACE ( 'NONE', ( #2096 ), #20296, .F. ) ;
#2431 = EDGE_LOOP ( 'NONE', ( #1647, #10781 ) ) ;
#2432 = EDGE_CURVE ( 'NONE', #18991, #13154, #12548, .T. ) ;
#2433 = CARTESIAN_POINT ( 'NONE',  ( 1.133692148550000001, -51.50000000000000000, -136.5552959530000123 ) ) ;
#2434 = CARTESIAN_POINT ( 'NONE',  ( -21.50145757605700325, 36.99754792876502307, -147.3684231709873416 ) ) ;
#2435 = PLANE ( 'NONE',  #1132 ) ;
#2436 = ORIENTED_EDGE ( 'NONE', *, *, #15852, .F. ) ;
#2437 = CARTESIAN_POINT ( 'NONE',  ( -12.08777119465849559, 36.07243015074993764, -148.3170434184952740 ) ) ;
#2438 = EDGE_CURVE ( 'NONE', #19256, #19447, #14586, .T. ) ;
#2439 = FACE_OUTER_BOUND ( 'NONE', #8276, .T. ) ;
#2440 = EDGE_CURVE ( 'NONE', #7436, #4448, #592, .T. ) ;
#2441 = CARTESIAN_POINT ( 'NONE',  ( -26.86963863710371925, 36.92213009831747428, -147.8538433455847496 ) ) ;
#2442 = LINE ( 'NONE', #9660, #21494 ) ;
#2443 = EDGE_CURVE ( 'NONE', #22710, #23189, #3641, .T. ) ;
#2444 = DIRECTION ( 'NONE',  ( 0.000000000000000000, -1.000000000000000000, -1.592654864069999939E-17 ) ) ;
#2445 = ORIENTED_EDGE ( 'NONE', *, *, #3029, .F. ) ;
#2446 = DIRECTION ( 'NONE',  ( 2.257144641399999941E-12, -4.009147065140000298E-51, 1.000000000000000000 ) ) ;
#2447 = VERTEX_POINT ( 'NONE', #1990 ) ;
#2448 = CARTESIAN_POINT ( 'NONE',  ( -13.88194885162993408, 32.82503397475245066, -144.7298409786526747 ) ) ;
#2449 = DIRECTION ( 'NONE',  ( 0.000000000000000000, 0.000000000000000000, 1.000000000000000000 ) ) ;
#2450 = CARTESIAN_POINT ( 'NONE',  ( -22.10824191589999899, -4.000000000000000000, -146.3157682190000060 ) ) ;
#2451 = ORIENTED_EDGE ( 'NONE', *, *, #16184, .F. ) ;
#2452 = CARTESIAN_POINT ( 'NONE',  ( 25.50000000000000000, 25.50000000000000000, -150.5552959529999839 ) ) ;
#2453 = DIRECTION ( 'NONE',  ( 2.257157423930000049E-12, 0.000000000000000000, 1.000000000000000000 ) ) ;
#2454 = VERTEX_POINT ( 'NONE', #16481 ) ;
#2455 = AXIS2_PLACEMENT_3D ( 'NONE', #5739, #10731, #23477 ) ;
#2456 = CARTESIAN_POINT ( 'NONE',  ( 9.695206431619142862, 37.90762969977967600, -141.7255920984417514 ) ) ;
#2457 = CARTESIAN_POINT ( 'NONE',  ( 7.310162460357136460, 36.08106663428162619, -146.3818244917397635 ) ) ;
#2458 = B_SPLINE_CURVE_WITH_KNOTS ( 'NONE', 5,
 ( #989, #17745, #1343, #21330, #22990, #15839, #6676, #23104, #14062, #11910, #5022, #4783 ),
 .UNSPECIFIED., .F., .F.,
 ( 6, 3, 3, 6 ),
 ( 0.000000000000000000, 4.454241660750000165, 8.943513424000000711, 13.47090878500000066 ),
 .UNSPECIFIED. ) ;
#2459 = EDGE_CURVE ( 'NONE', #3522, #17914, #14792, .T. ) ;
#2460 = PLANE ( 'NONE',  #7430 ) ;
#2461 = EDGE_CURVE ( 'NONE', #5202, #15683, #6236, .T. ) ;
#2462 = CARTESIAN_POINT ( 'NONE',  ( 32.00000000010000178, -33.03620104880000241, -136.0552959530000123 ) ) ;
#2463 = ORIENTED_EDGE ( 'NONE', *, *, #23431, .F. ) ;
#2464 = CARTESIAN_POINT ( 'NONE',  ( -35.47299999999999898, 14.00000000000000000, -144.0552959529999839 ) ) ;
#2465 = ORIENTED_EDGE ( 'NONE', *, *, #8630, .T. ) ;
#2466 = CARTESIAN_POINT ( 'NONE',  ( -21.35824191589999899, -32.00000000000000000, -144.8157682190000060 ) ) ;
#2467 = ORIENTED_EDGE ( 'NONE', *, *, #1151, .F. ) ;
#2468 = DIRECTION ( 'NONE',  ( 0.000000000000000000, 1.000000000000000000, 0.000000000000000000 ) ) ;
#2469 = ORIENTED_EDGE ( 'NONE', *, *, #18997, .F. ) ;
#2470 = CARTESIAN_POINT ( 'NONE',  ( -23.34852387253397765, 35.17565678551333974, -140.0195222351592861 ) ) ;
#2471 = EDGE_LOOP ( 'NONE', ( #2009, #23532, #9432, #9647 ) ) ;
#2472 = CARTESIAN_POINT ( 'NONE',  ( -14.21475634692214740, -45.92191803000493877, -150.0552959529999839 ) ) ;
#2473 = ORIENTED_EDGE ( 'NONE', *, *, #19713, .T. ) ;
#2474 = ORIENTED_EDGE ( 'NONE', *, *, #19892, .T. ) ;
#2475 = CARTESIAN_POINT ( 'NONE',  ( -27.50477442134641493, 37.98689587843293936, -148.6879642405163224 ) ) ;
#2476 = CARTESIAN_POINT ( 'NONE',  ( -14.83278250959999944, 40.60058613829999530, -144.4189779529999953 ) ) ;
#2477 = LINE ( 'NONE', #20215, #22509 ) ;
#2478 = DIRECTION ( 'NONE',  ( 0.000000000000000000, 1.000000000000000000, 0.000000000000000000 ) ) ;
#2479 = CARTESIAN_POINT ( 'NONE',  ( -7.506111428155179510, 33.37436714669472337, -146.3147224701790208 ) ) ;
#2480 = EDGE_LOOP ( 'NONE', ( #6252, #957, #9033, #21625 ) ) ;
#2481 = CARTESIAN_POINT ( 'NONE',  ( 4.500000000000000000, -3.500000000000000000, -145.5552959529999839 ) ) ;
#2482 = ADVANCED_FACE ( 'NONE', ( #20760 ), #7663, .T. ) ;
#2483 = ADVANCED_FACE ( 'NONE', ( #2557 ), #424, .T. ) ;
#2484 = VECTOR ( 'NONE', #21541, 1000.000000000000114 ) ;
#2485 = CARTESIAN_POINT ( 'NONE',  ( -24.22314457607385663, 36.96432676151306396, -148.6204621725955235 ) ) ;
#2486 = EDGE_CURVE ( 'NONE', #6697, #2330, #18740, .T. ) ;
#2487 = ORIENTED_EDGE ( 'NONE', *, *, #4265, .T. ) ;
#2488 = CARTESIAN_POINT ( 'NONE',  ( -13.01389323884992066, 37.83362044807778801, -147.7995900185891003 ) ) ;
#2489 = CARTESIAN_POINT ( 'NONE',  ( 19.13369214859999801, -51.50000000000000000, -143.0552959529999839 ) ) ;
#2490 = CARTESIAN_POINT ( 'NONE',  ( -23.41786221899999987, 36.12684018730000446, -140.1150171360000058 ) ) ;
#2491 = ORIENTED_EDGE ( 'NONE', *, *, #19317, .F. ) ;
#2492 = LINE ( 'NONE', #9367, #4851 ) ;
#2493 = LINE ( 'NONE', #13417, #5918 ) ;
#2494 = VERTEX_POINT ( 'NONE', #2450 ) ;
#2495 = UNCERTAINTY_MEASURE_WITH_UNIT (LENGTH_MEASURE( 1.000000000000000082E-05 ), #9901, 'distance_accuracy_value', 'NONE');
#2496 = CARTESIAN_POINT ( 'NONE',  ( 25.31684607480000082, -45.26810052400000473, -149.5552959529999839 ) ) ;
#2497 = FACE_OUTER_BOUND ( 'NONE', #23066, .T. ) ;
#2498 = EDGE_LOOP ( 'NONE', ( #6112, #12899, #5310, #14689 ) ) ;
#2499 = DIRECTION ( 'NONE',  ( -0.9949850929136110356, 0.1000233216789610247, -7.446425804567087094E-15 ) ) ;
#2500 = CARTESIAN_POINT ( 'NONE',  ( -20.36280570458463757, 40.92149091583824116, -144.5882336176433967 ) ) ;
#2501 = ORIENTED_EDGE ( 'NONE', *, *, #6823, .T. ) ;
#2502 = CARTESIAN_POINT ( 'NONE',  ( -27.69172573212000543, 35.55337010885431681, -147.2624953929817480 ) ) ;
#2503 = CARTESIAN_POINT ( 'NONE',  ( 23.50000000000000000, -20.50000000000000000, -136.0552959530000123 ) ) ;
#2504 = EDGE_LOOP ( 'NONE', ( #2554, #7882, #8397, #3230 ) ) ;
#2505 = CARTESIAN_POINT ( 'NONE',  ( 6.750000000030000002, -44.75000000000000000, -136.0552959530000123 ) ) ;
#2506 = VECTOR ( 'NONE', #7045, 1000.000000000000114 ) ;
#2507 = LINE ( 'NONE', #4393, #4653 ) ;
#2508 = AXIS2_PLACEMENT_3D ( 'NONE', #14330, #17666, #10499 ) ;
#2509 = CARTESIAN_POINT ( 'NONE',  ( -10.75221293960000146, 33.20739279120000020, -143.4848104349999858 ) ) ;
#2510 = EDGE_LOOP ( 'NONE', ( #11261, #16222, #18656, #11978 ) ) ;
#2511 = CARTESIAN_POINT ( 'NONE',  ( -3.499999999949999996, 40.00000000000000000, -150.0552959529999839 ) ) ;
#2512 = CARTESIAN_POINT ( 'NONE',  ( -1.898424454282724216, 45.72687021304442112, -136.0552959529957207 ) ) ;
#2513 = VERTEX_POINT ( 'NONE', #13485 ) ;
#2514 = EDGE_CURVE ( 'NONE', #19622, #8290, #8123, .T. ) ;
#2515 = EDGE_CURVE ( 'NONE', #12071, #8946, #22656, .T. ) ;
#2516 = VERTEX_POINT ( 'NONE', #22303 ) ;
#2517 = DIRECTION ( 'NONE',  ( 1.000000000000000000, 0.000000000000000000, 2.516505522483685870E-12 ) ) ;
#2518 = LINE ( 'NONE', #14890, #203 ) ;
#2519 = CARTESIAN_POINT ( 'NONE',  ( 3.611688725869999975E-11, 25.50000000000000000, -136.0552959530000123 ) ) ;
#2520 = ORIENTED_EDGE ( 'NONE', *, *, #19556, .F. ) ;
#2521 = DIRECTION ( 'NONE',  ( -2.257144641399999941E-12, 8.049635416090000264E-35, -1.000000000000000000 ) ) ;
#2522 = AXIS2_PLACEMENT_3D ( 'NONE', #14920, #19074, #18835 ) ;
#2523 = CARTESIAN_POINT ( 'NONE',  ( 8.633772787769999013, -29.00605602609999778, -147.5552959529999839 ) ) ;
#2524 = DIRECTION ( 'NONE',  ( 0.000000000000000000, 0.000000000000000000, 1.000000000000000000 ) ) ;
#2525 = CARTESIAN_POINT ( 'NONE',  ( -4.500000000000000000, 0.000000000000000000, -150.0552959529999839 ) ) ;
#2526 = LINE ( 'NONE', #9748, #2248 ) ;
#2527 = ADVANCED_FACE ( 'NONE', ( #11686 ), #19088, .T. ) ;
#2528 = CARTESIAN_POINT ( 'NONE',  ( -4.499999999959999109, 34.00000000000000000, -136.0552959530000123 ) ) ;
#2529 = CARTESIAN_POINT ( 'NONE',  ( -17.22605506639999717, 36.97564272059999979, -139.5994799229999899 ) ) ;
#2530 = FACE_OUTER_BOUND ( 'NONE', #18422, .T. ) ;
#2531 = DIRECTION ( 'NONE',  ( 2.257144641404620116E-12, 2.777754792983395132E-24, 1.000000000000000000 ) ) ;
#2532 = CARTESIAN_POINT ( 'NONE',  ( 6.000000000000000000, -3.500000000000000000, -140.0552959529999839 ) ) ;
#2533 = EDGE_CURVE ( 'NONE', #17699, #13091, #2085, .T. ) ;
#2534 = ORIENTED_EDGE ( 'NONE', *, *, #14317, .T. ) ;
#2535 = CARTESIAN_POINT ( 'NONE',  ( -9.518386210255387780, 33.60980554410204491, -145.7502876509803684 ) ) ;
#2536 = PLANE ( 'NONE',  #5799 ) ;
#2537 = ORIENTED_EDGE ( 'NONE', *, *, #5328, .F. ) ;
#2538 = DIRECTION ( 'NONE',  ( 0.000000000000000000, -1.000000000000000000, 0.000000000000000000 ) ) ;
#2539 = CARTESIAN_POINT ( 'NONE',  ( -22.27877656138748463, 35.45284992532844370, -147.6448678430727455 ) ) ;
#2540 = ADVANCED_FACE ( 'NONE', ( #899 ), #4099, .F. ) ;
#2541 = DIRECTION ( 'NONE',  ( 0.000000000000000000, 1.000000000000000000, 0.000000000000000000 ) ) ;
#2542 = ORIENTED_EDGE ( 'NONE', *, *, #3842, .T. ) ;
#2543 = CARTESIAN_POINT ( 'NONE',  ( -12.02450515624455640, 36.94061592734299637, -147.5849826166407013 ) ) ;
#2544 = PLANE ( 'NONE',  #4410 ) ;
#2545 = CARTESIAN_POINT ( 'NONE',  ( -14.93328160137761706, 36.92972691758931347, -148.3740393307602972 ) ) ;
#2546 = CARTESIAN_POINT ( 'NONE',  ( -7.500000000000000000, 42.50000000000000000, -150.5552959529999839 ) ) ;
#2547 = CARTESIAN_POINT ( 'NONE',  ( -34.35824191590000254, -18.00000000000000000, -150.0657682190000060 ) ) ;
#2548 = CARTESIAN_POINT ( 'NONE',  ( -8.613431449198317935, 37.75849558882340062, -140.1079839310028206 ) ) ;
#2549 = EDGE_CURVE ( 'NONE', #21164, #3612, #9668, .T. ) ;
#2550 = ORIENTED_EDGE ( 'NONE', *, *, #13380, .F. ) ;
#2551 = AXIS2_PLACEMENT_3D ( 'NONE', #16524, #346, #3681 ) ;
#2552 = CARTESIAN_POINT ( 'NONE',  ( -21.35824191589999899, -32.00000000000000000, -144.8157682190000060 ) ) ;
#2553 = APPLICATION_PROTOCOL_DEFINITION ( 'draft international standard', 'automotive_design', 1998, #2202 ) ;
#2554 = ORIENTED_EDGE ( 'NONE', *, *, #15296, .F. ) ;
#2555 = CARTESIAN_POINT ( 'NONE',  ( -14.03815736070903597, 32.86934428549125187, -141.8938335452860997 ) ) ;
#2556 = CARTESIAN_POINT ( 'NONE',  ( 13.13369214870000157, -2.273736754430000208E-12, -136.0552959530000123 ) ) ;
#2557 = FACE_OUTER_BOUND ( 'NONE', #10683, .T. ) ;
#2558 = EDGE_CURVE ( 'NONE', #5708, #19622, #18777, .T. ) ;
#2559 = VERTEX_POINT ( 'NONE', #652 ) ;
#2560 = LINE ( 'NONE', #17417, #19780 ) ;
#2561 = DIRECTION ( 'NONE',  ( -1.000000000000000000, 0.000000000000000000, 2.257120985840000117E-12 ) ) ;
#2562 = EDGE_CURVE ( 'NONE', #2284, #2706, #19153, .T. ) ;
#2563 = ORIENTED_EDGE ( 'NONE', *, *, #18776, .T. ) ;
#2564 = CARTESIAN_POINT ( 'NONE',  ( -21.02182045561234247, 40.23839372147724447, -142.1761255659782250 ) ) ;
#2565 = EDGE_CURVE ( 'NONE', #19064, #7036, #17058, .T. ) ;
#2566 = AXIS2_PLACEMENT_3D ( 'NONE', #21950, #11323, #3862 ) ;
#2567 = EDGE_CURVE ( 'NONE', #5894, #1590, #22425, .T. ) ;
#2568 = CARTESIAN_POINT ( 'NONE',  ( -18.19668323639750440, 39.07774783162744825, -146.8458198118272549 ) ) ;
#2569 = MECHANICAL_DESIGN_GEOMETRIC_PRESENTATION_REPRESENTATION (  '', ( #19668 ), #23454 ) ;
#2570 = CARTESIAN_POINT ( 'NONE',  ( 7.204510097230632404, 37.75811448146659188, -146.4379907056525951 ) ) ;
#2571 = CARTESIAN_POINT ( 'NONE',  ( -23.51619327739999932, 36.94101002280000046, -140.1031831869999849 ) ) ;
#2572 = CARTESIAN_POINT ( 'NONE',  ( -24.94615679292102683, 36.31107517788785799, -147.5592587911377791 ) ) ;
#2573 = EDGE_LOOP ( 'NONE', ( #11204, #11882, #8757, #13422 ) ) ;
#2574 = DIRECTION ( 'NONE',  ( -2.602084704489999637E-17, 1.000000000000000000, 0.000000000000000000 ) ) ;
#2575 = ORIENTED_EDGE ( 'NONE', *, *, #11511, .T. ) ;
#2576 = CARTESIAN_POINT ( 'NONE',  ( -34.50000000000000000, -64.50000000000000000, -144.0552959529999839 ) ) ;
#2578 = EDGE_LOOP ( 'NONE', ( #16493, #15663, #9579, #17088 ) ) ;
#2577 = AXIS2_PLACEMENT_3D ( 'NONE', #69, #14579, #6516 ) ;
#2579 = DIRECTION ( 'NONE',  ( 0.000000000000000000, -1.000000000000000000, 0.000000000000000000 ) ) ;
#2580 = VERTEX_POINT ( 'NONE', #5994 ) ;
#2581 = LINE ( 'NONE', #22565, #7194 ) ;
#2582 = VECTOR ( 'NONE', #19877, 1000.000000000000000 ) ;
#2583 = ORIENTED_EDGE ( 'NONE', *, *, #15352, .F. ) ;
#2584 = DIRECTION ( 'NONE',  ( 0.000000000000000000, 6.264364525598899972E-11, -1.000000000000000000 ) ) ;
#2585 = ORIENTED_EDGE ( 'NONE', *, *, #14036, .F. ) ;
#2586 = ORIENTED_EDGE ( 'NONE', *, *, #344, .F. ) ;
#2587 = CARTESIAN_POINT ( 'NONE',  ( -27.39837063315040311, 38.96261900911265030, -148.4292450421148715 ) ) ;
#2588 = CARTESIAN_POINT ( 'NONE',  ( -18.35824191589999899, -18.00000000000000000, -141.0657682190000060 ) ) ;
#2589 = EDGE_CURVE ( 'NONE', #15557, #23525, #13250, .T. ) ;
#2590 = CARTESIAN_POINT ( 'NONE',  ( -10.79374130943622134, 37.77220497676849931, -140.6646249280453844 ) ) ;
#2591 = CARTESIAN_POINT ( 'NONE',  ( -6.472921198530737996, 34.24272888346551724, -147.8944248432848099 ) ) ;
#2592 = CARTESIAN_POINT ( 'NONE',  ( -9.302015002957228162, 41.36125941937655881, -143.4861728416109088 ) ) ;
#2593 = ORIENTED_EDGE ( 'NONE', *, *, #20659, .T. ) ;
#2594 = DIRECTION ( 'NONE',  ( -0.9848077530125625145, 0.000000000000000000, -0.1736481776649201891 ) ) ;
#2595 = VECTOR ( 'NONE', #11326, 1000.000000000000000 ) ;
#2596 = CARTESIAN_POINT ( 'NONE',  ( -14.70358821722507159, 36.91864139955099233, -140.0875527721395599 ) ) ;
#2597 = AXIS2_PLACEMENT_3D ( 'NONE', #20775, #15306, #8139 ) ;
#2598 = PLANE ( 'NONE',  #20129 ) ;
#2599 = EDGE_LOOP ( 'NONE', ( #16523, #22024, #4791, #18185 ) ) ;
#2600 = CARTESIAN_POINT ( 'NONE',  ( -18.35824191589999899, -34.50000000000000000, -146.3157682190000060 ) ) ;
#2601 = LINE ( 'NONE', #13298, #1208 ) ;
#2602 = VERTEX_POINT ( 'NONE', #4338 ) ;
#2603 = DIRECTION ( 'NONE',  ( 1.211690350419999855E-27, 2.765629237170000203E-27, -1.000000000000000000 ) ) ;
#2604 = CARTESIAN_POINT ( 'NONE',  ( -18.07392865170000107, -18.00000000000000000, -147.3157682190000060 ) ) ;
#2605 = ORIENTED_EDGE ( 'NONE', *, *, #15186, .F. ) ;
#2606 = CARTESIAN_POINT ( 'NONE',  ( -21.12162747683233377, 36.95220905038714676, -147.5578847870536947 ) ) ;
#2607 = CARTESIAN_POINT ( 'NONE',  ( 31.50000000020000002, -40.03620104850000416, -136.0552959530000123 ) ) ;
#2608 = ORIENTED_EDGE ( 'NONE', *, *, #16527, .T. ) ;
#2609 = PLANE ( 'NONE',  #8684 ) ;
#2610 = CARTESIAN_POINT ( 'NONE',  ( -19.54668701386443885, 37.05673630843094202, -139.5622637237091226 ) ) ;
#2611 = ORIENTED_EDGE ( 'NONE', *, *, #6655, .F. ) ;
#2612 = SHAPE_REPRESENTATION_RELATIONSHIP ( 'NONE' , 'NONE' ,  #538, #22005 ) ;
#2613 = CARTESIAN_POINT ( 'NONE',  ( -28.37659674026075862, 36.31875307945076514, -140.4290075092151824 ) ) ;
#2614 = VECTOR ( 'NONE', #12850, 1000.000000000000000 ) ;
#2615 = CARTESIAN_POINT ( 'NONE',  ( -14.47770030809999930, -1.500000000000000000, -148.5552959529999839 ) ) ;
#2616 = AXIS2_PLACEMENT_3D ( 'NONE', #16622, #7578, #14853 ) ;
#2617 = ADVANCED_FACE ( 'NONE', ( #780 ), #11571, .T. ) ;
#2618 = VERTEX_POINT ( 'NONE', #5148 ) ;
#2619 = CARTESIAN_POINT ( 'NONE',  ( 12.01554901919999985, -37.47280209340000567, -145.0552959529999839 ) ) ;
#2620 = VECTOR ( 'NONE', #14874, 1000.000000000000000 ) ;
#2621 = DIRECTION ( 'NONE',  ( -1.211690350419999855E-27, -2.765629237170000203E-27, 1.000000000000000000 ) ) ;
#2622 = VERTEX_POINT ( 'NONE', #21357 ) ;
#2623 = CARTESIAN_POINT ( 'NONE',  ( -10.17933436569999905, 35.38122503049999779, -147.6311798959999919 ) ) ;
#2624 = VERTEX_POINT ( 'NONE', #15862 ) ;
#2625 = VECTOR ( 'NONE', #22025, 1000.000000000000000 ) ;
#2626 = CARTESIAN_POINT ( 'NONE',  ( -35.20609992760000040, 16.68710169819999933, -143.5552959529999839 ) ) ;
#2627 = FACE_OUTER_BOUND ( 'NONE', #22702, .T. ) ;
#2628 = VERTEX_POINT ( 'NONE', #4809 ) ;
#2629 = ORIENTED_EDGE ( 'NONE', *, *, #11125, .F. ) ;
#2630 = DIRECTION ( 'NONE',  ( 1.000000000000000000, 0.000000000000000000, -8.953948693601887499E-12 ) ) ;
#2631 = VECTOR ( 'NONE', #11038, 1000.000000000000000 ) ;
#2632 = DIRECTION ( 'NONE',  ( -2.257144641399999941E-12, 4.009147065140000298E-51, -1.000000000000000000 ) ) ;
#2633 = AXIS2_PLACEMENT_3D ( 'NONE', #18178, #17947, #8883 ) ;
#2634 = CARTESIAN_POINT ( 'NONE',  ( -13.73025257492641060, 37.03482478361183183, -140.6242165752723565 ) ) ;
#2635 = LINE ( 'NONE', #20712, #22030 ) ;
#2636 = ORIENTED_EDGE ( 'NONE', *, *, #18562, .T. ) ;
#2637 = DIRECTION ( 'NONE',  ( 1.000000000000000000, 0.000000000000000000, 0.000000000000000000 ) ) ;
#2638 = DIRECTION ( 'NONE',  ( -0.4567501391959232770, -0.5397956190499111351, 0.7071067811858601226 ) ) ;
#2639 = AXIS2_PLACEMENT_3D ( 'NONE', #2619, #599, #7606 ) ;
#2640 = CARTESIAN_POINT ( 'NONE',  ( -16.50000000000000000, -43.00000000000000000, -150.0552959529999839 ) ) ;
#2641 = DIRECTION ( 'NONE',  ( -2.257157423930000049E-12, 0.000000000000000000, -1.000000000000000000 ) ) ;
#2642 = VECTOR ( 'NONE', #3185, 1000.000000000000000 ) ;
#2643 = CARTESIAN_POINT ( 'NONE',  ( -24.11597423730821177, 41.68006656443377267, -143.5803335156247158 ) ) ;
#2644 = CARTESIAN_POINT ( 'NONE',  ( -16.54277457355827963, 34.95491693754559748, -141.0331736024876079 ) ) ;
#2645 = EDGE_CURVE ( 'NONE', #2031, #1998, #3255, .T. ) ;
#2646 = CARTESIAN_POINT ( 'NONE',  ( -9.999999999959999997, 42.50000000000000000, -136.0552959530000123 ) ) ;
#2647 = CARTESIAN_POINT ( 'NONE',  ( -20.45144833149999997, 36.94873838139999833, -139.8044047869999815 ) ) ;
#2648 = DIRECTION ( 'NONE',  ( 1.000000000000000000, 0.000000000000000000, 0.000000000000000000 ) ) ;
#2649 = EDGE_CURVE ( 'NONE', #1861, #6185, #21333, .T. ) ;
#2650 = LINE ( 'NONE', #2184, #14973 ) ;
#2651 = ORIENTED_EDGE ( 'NONE', *, *, #18429, .F. ) ;
#2652 = CARTESIAN_POINT ( 'NONE',  ( -9.944031889410000602, 32.62729151690000151, -143.2983400859999961 ) ) ;
#2653 = APPLICATION_CONTEXT ( 'automotive_design' ) ;
#2654 = VECTOR ( 'NONE', #22857, 1000.000000000000000 ) ;
#2655 = DIRECTION ( 'NONE',  ( 0.000000000000000000, 1.000000000000000000, 0.000000000000000000 ) ) ;
#2656 = ORIENTED_EDGE ( 'NONE', *, *, #4863, .T. ) ;
#2657 = VECTOR ( 'NONE', #14851, 1000.000000000000227 ) ;
#2658 = CIRCLE ( 'NONE', #13264, 7.499999999999999112 ) ;
#2659 = AXIS2_PLACEMENT_3D ( 'NONE', #8598, #14328, #6710 ) ;
#2660 = CARTESIAN_POINT ( 'NONE',  ( -21.99818215266191501, 36.31189858315303098, -147.5072904936844509 ) ) ;
#2661 = LINE ( 'NONE', #4432, #22029 ) ;
#2662 = ORIENTED_EDGE ( 'NONE', *, *, #9008, .T. ) ;
#2663 = CARTESIAN_POINT ( 'NONE',  ( -24.21201708719999957, 40.99356323119999956, -143.6328343570000072 ) ) ;
#2664 = DIRECTION ( 'NONE',  ( 2.839308199620000013E-14, 3.568879590630000244E-13, 1.000000000000000000 ) ) ;
#2665 = CARTESIAN_POINT ( 'NONE',  ( 6.500000000170000014, 20.50000000000000000, -136.5552959530000123 ) ) ;
#2666 = CARTESIAN_POINT ( 'NONE',  ( 25.00000852249999994, -26.83294714660000224, -143.5552959529999839 ) ) ;
#2667 = CARTESIAN_POINT ( 'NONE',  ( 8.900000000049999471, 39.46779253580000102, -149.1552959530000066 ) ) ;
#2668 = DIRECTION ( 'NONE',  ( -1.000000000000000000, 0.000000000000000000, 0.000000000000000000 ) ) ;
#2669 = EDGE_CURVE ( 'NONE', #9439, #4983, #11932, .T. ) ;
#2670 = CARTESIAN_POINT ( 'NONE',  ( 9.736704675116099494, -36.41257638424534093, -150.0552959529999555 ) ) ;
#2671 = ORIENTED_EDGE ( 'NONE', *, *, #7178, .T. ) ;
#2672 = VECTOR ( 'NONE', #5152, 1000.000000000000000 ) ;
#2673 = AXIS2_PLACEMENT_3D ( 'NONE', #21992, #7464, #12464 ) ;
#2674 = CARTESIAN_POINT ( 'NONE',  ( -28.00347998531936966, 37.05747243975231697, -148.5422211674587629 ) ) ;
#2675 = VECTOR ( 'NONE', #17204, 1000.000000000000000 ) ;
#2676 = ORIENTED_EDGE ( 'NONE', *, *, #13478, .F. ) ;
#2677 = CARTESIAN_POINT ( 'NONE',  ( -14.03631397270657999, 35.00148697007204390, -139.7760274526582407 ) ) ;
#2678 = CARTESIAN_POINT ( 'NONE',  ( -25.64792992860000354, 37.04465132570000208, -139.7265440090000084 ) ) ;
#2679 = ADVANCED_FACE ( 'NONE', ( #15987 ), #21468, .F. ) ;
#2680 = CARTESIAN_POINT ( 'NONE',  ( -5.070907855429999778, -22.41528233759999722, -147.5552959529999839 ) ) ;
#2681 = ORIENTED_EDGE ( 'NONE', *, *, #18120, .T. ) ;
#2682 = DIRECTION ( 'NONE',  ( 1.000000000000000000, -1.190078432789999897E-50, -2.257144641399999941E-12 ) ) ;
#2683 = CARTESIAN_POINT ( 'NONE',  ( -14.02405267930000043, 37.94700976039999318, -139.5674429869999926 ) ) ;
#2684 = VERTEX_POINT ( 'NONE', #12289 ) ;
#2685 = CARTESIAN_POINT ( 'NONE',  ( -4.499999999969999109, 34.00000000000000000, -137.0552959530000123 ) ) ;
#2686 = EDGE_CURVE ( 'NONE', #16611, #20903, #6473, .T. ) ;
#2687 = CARTESIAN_POINT ( 'NONE',  ( -18.64767072899999789, 38.89869937459999960, -148.1651290810000319 ) ) ;
#2688 = VECTOR ( 'NONE', #6527, 1000.000000000000000 ) ;
#2689 = CARTESIAN_POINT ( 'NONE',  ( 7.202503882904777832, 36.24063282234246230, -146.4386832613703575 ) ) ;
#2690 = AXIS2_PLACEMENT_3D ( 'NONE', #6355, #904, #19094 ) ;
#2691 = DIRECTION ( 'NONE',  ( 0.000000000000000000, -1.000000000000000000, 0.000000000000000000 ) ) ;
#2692 = CARTESIAN_POINT ( 'NONE',  ( -26.10314130450000292, 34.70878586860000325, -141.0128996759999893 ) ) ;
#2693 = DIRECTION ( 'NONE',  ( -1.000000000000000000, 0.000000000000000000, 0.000000000000000000 ) ) ;
#2694 = EDGE_CURVE ( 'NONE', #13175, #11596, #10273, .T. ) ;
#2695 = ADVANCED_FACE ( 'NONE', ( #1014 ), #8590, .T. ) ;
#2696 = ORIENTED_EDGE ( 'NONE', *, *, #1439, .T. ) ;
#2697 = CARTESIAN_POINT ( 'NONE',  ( 31.00000000000000000, -39.80430157320000006, -150.0552959529999839 ) ) ;
#2698 = EDGE_CURVE ( 'NONE', #7704, #15634, #13963, .T. ) ;
#2699 = ORIENTED_EDGE ( 'NONE', *, *, #22898, .F. ) ;
#2700 = VERTEX_POINT ( 'NONE', #8706 ) ;
#2701 = CARTESIAN_POINT ( 'NONE',  ( -15.00000000000000000, -43.00000000000000000, -145.5552959529999839 ) ) ;
#2702 = EDGE_CURVE ( 'NONE', #12619, #11114, #14202, .T. ) ;
#2703 = ORIENTED_EDGE ( 'NONE', *, *, #14053, .F. ) ;
#2704 = CARTESIAN_POINT ( 'NONE',  ( 6.007013984479645963, 28.00000000000003197, -136.0552959530135979 ) ) ;
#2705 = VECTOR ( 'NONE', #14475, 1000.000000000000000 ) ;
#2706 = VERTEX_POINT ( 'NONE', #22773 ) ;
#2707 = VECTOR ( 'NONE', #21869, 1000.000000000000000 ) ;
#2708 = VECTOR ( 'NONE', #16689, 1000.000000000000000 ) ;
#2709 = ORIENTED_EDGE ( 'NONE', *, *, #18836, .T. ) ;
#2710 = DIRECTION ( 'NONE',  ( 0.000000000000000000, -1.000000000000000000, 0.000000000000000000 ) ) ;
#2711 = DIRECTION ( 'NONE',  ( -0.9892101392001054760, 0.1465035852930155480, 4.471489433380478225E-12 ) ) ;
#2712 = CARTESIAN_POINT ( 'NONE',  ( -10.74479785762736661, 39.62990750194220624, -140.6987230986796078 ) ) ;
#2713 = CARTESIAN_POINT ( 'NONE',  ( -22.10824191589623311, -3.803650459151263874, -146.3157682190000344 ) ) ;
#2714 = CARTESIAN_POINT ( 'NONE',  ( -8.514310886030200365, 36.94123471670563674, -140.1199228274903987 ) ) ;
#2715 = CARTESIAN_POINT ( 'NONE',  ( -9.008354782749020018, 41.28660893102239982, -146.4928760736580386 ) ) ;
#2716 = VERTEX_POINT ( 'NONE', #23128 ) ;
#2717 = EDGE_CURVE ( 'NONE', #19898, #18293, #13851, .T. ) ;
#2718 = CARTESIAN_POINT ( 'NONE',  ( 9.948241962799819760, 37.39437665988412363, -146.5244709269353791 ) ) ;
#2719 = DIRECTION ( 'NONE',  ( -1.000000000000000000, 5.094701932209999624E-24, 2.257144641399999941E-12 ) ) ;
#2720 = VECTOR ( 'NONE', #5141, 1000.000000000000000 ) ;
#2721 = ORIENTED_EDGE ( 'NONE', *, *, #8082, .T. ) ;
#2722 = AXIS2_PLACEMENT_3D ( 'NONE', #3581, #6907, #3225 ) ;
#2723 = ADVANCED_FACE ( 'NONE', ( #1138 ), #8368, .F. ) ;
#2724 = EDGE_CURVE ( 'NONE', #1140, #23501, #6701, .T. ) ;
#2725 = CARTESIAN_POINT ( 'NONE',  ( -18.12563077678109380, 37.94526991178427977, -148.6669620614958944 ) ) ;
#2726 = CYLINDRICAL_SURFACE ( 'NONE', #2340, 0.5000000000000004441 ) ;
#2727 = ORIENTED_EDGE ( 'NONE', *, *, #18960, .F. ) ;
#2728 = LINE ( 'NONE', #2835, #13984 ) ;
#2729 = FACE_OUTER_BOUND ( 'NONE', #12220, .T. ) ;
#2730 = ORIENTED_EDGE ( 'NONE', *, *, #7098, .F. ) ;
#2731 = CARTESIAN_POINT ( 'NONE',  ( -38.50000000000000000, 47.50000000000000000, -149.5552959529999839 ) ) ;
#2732 = CARTESIAN_POINT ( 'NONE',  ( -18.53945141080000170, 39.74065879090000664, -147.6687609889999919 ) ) ;
#2733 = ORIENTED_EDGE ( 'NONE', *, *, #21429, .T. ) ;
#2734 = CARTESIAN_POINT ( 'NONE',  ( -15.39088246931257942, 40.97264801224785913, -143.5343598390859938 ) ) ;
#2735 = CARTESIAN_POINT ( 'NONE',  ( -24.83693579151085373, 35.06568064903114390, -148.4846062725258662 ) ) ;
#2736 = EDGE_LOOP ( 'NONE', ( #3472, #17792 ) ) ;
#2737 =( NAMED_UNIT ( * ) SI_UNIT ( $, .STERADIAN. ) SOLID_ANGLE_UNIT ( ) );
#2738 = CARTESIAN_POINT ( 'NONE',  ( -3.499999999959999997, 34.00000000000000000, -136.0552959530000123 ) ) ;
#2739 = EDGE_LOOP ( 'NONE', ( #2798, #6479, #6612, #20977, #6785, #22477, #16616, #17206 ) ) ;
#2740 = FACE_OUTER_BOUND ( 'NONE', #2504, .T. ) ;
#2741 = DIRECTION ( 'NONE',  ( 1.526468026909999897E-13, 8.159623473500000156E-13, 1.000000000000000000 ) ) ;
#2742 = ORIENTED_EDGE ( 'NONE', *, *, #7932, .T. ) ;
#2743 = CARTESIAN_POINT ( 'NONE',  ( -32.50000000000000000, -51.00000000000000000, -149.5552959529999839 ) ) ;
#2744 = AXIS2_PLACEMENT_3D ( 'NONE', #22872, #2531, #4664 ) ;
#2745 = VECTOR ( 'NONE', #15481, 1000.000000000000000 ) ;
#2746 = EDGE_LOOP ( 'NONE', ( #14652, #1260, #8463, #21117 ) ) ;
#2747 = CARTESIAN_POINT ( 'NONE',  ( -35.33948162989999986, 11.17737245070000185, -143.5552959529999839 ) ) ;
#2748 = DIRECTION ( 'NONE',  ( -2.257144641399999941E-12, 0.000000000000000000, -1.000000000000000000 ) ) ;
#2749 = EDGE_LOOP ( 'NONE', ( #13497, #10323 ) ) ;
#2750 = VERTEX_POINT ( 'NONE', #12175 ) ;
#2751 = CARTESIAN_POINT ( 'NONE',  ( 7.500000000000000888, -3.107300918301275416, -150.0552959530000123 ) ) ;
#2752 = B_SPLINE_CURVE_WITH_KNOTS ( 'NONE', 3,
 ( #5830, #9622, #495, #8078, #18799, #11177, #20596, #18915, #20705, #17131 ),
 .UNSPECIFIED., .F., .F.,
 ( 4, 2, 2, 2, 4 ),
 ( 0.000000000000000000, 0.2499999999999985012, 0.4999999999999990008, 0.7499999999999994449, 1.000000000000000000 ),
 .UNSPECIFIED. ) ;
#2753 = EDGE_CURVE ( 'NONE', #16256, #6145, #3615, .T. ) ;
#2754 = CARTESIAN_POINT ( 'NONE',  ( -20.95225485091065565, 36.93199168240901997, -148.3394883768439740 ) ) ;
#2755 = EDGE_CURVE ( 'NONE', #16273, #2844, #19674, .T. ) ;
#2756 = CARTESIAN_POINT ( 'NONE',  ( 19.04211518569999839, -51.50000000000000000, -150.0552959529999839 ) ) ;
#2757 = FACE_OUTER_BOUND ( 'NONE', #2887, .T. ) ;
#2758 = VERTEX_POINT ( 'NONE', #1960 ) ;
#2759 = AXIS2_PLACEMENT_3D ( 'NONE', #1416, #14369, #1306 ) ;
#2760 = DIRECTION ( 'NONE',  ( -7.367827251323790032E-12, 0.000000000000000000, -1.000000000000000000 ) ) ;
#2761 = AXIS2_PLACEMENT_3D ( 'NONE', #16975, #2023, #14961 ) ;
#2762 = PLANE ( 'NONE',  #20444 ) ;
#2763 = DIRECTION ( 'NONE',  ( -0.9874789572432817186, 0.1577507813030449846, 2.479216961550704427E-14 ) ) ;
#2764 = LINE ( 'NONE', #19166, #18192 ) ;
#2765 = ORIENTED_EDGE ( 'NONE', *, *, #16235, .F. ) ;
#2766 = DIRECTION ( 'NONE',  ( -0.7071067811865474617, 0.7071067811865475727, 0.000000000000000000 ) ) ;
#2767 = CARTESIAN_POINT ( 'NONE',  ( -17.10416939857909213, 33.74918808323167241, -142.0823092718280805 ) ) ;
#2768 = LINE ( 'NONE', #1454, #11832 ) ;
#2769 = CARTESIAN_POINT ( 'NONE',  ( 7.228490359739999427, -13.33508289800000135, -146.5552959529999839 ) ) ;
#2770 = CARTESIAN_POINT ( 'NONE',  ( 0.3832000607639999834, -34.50000000000000000, -150.0552959529999839 ) ) ;
#2771 = ORIENTED_EDGE ( 'NONE', *, *, #225, .T. ) ;
#2772 = PLANE ( 'NONE',  #11 ) ;
#2773 = CARTESIAN_POINT ( 'NONE',  ( -29.62481956326176658, 40.87340935581828205, -146.3463541501877785 ) ) ;
#2774 = CARTESIAN_POINT ( 'NONE',  ( -32.50000000000000000, 19.50000000020000002, -137.0552959530000123 ) ) ;
#2775 = EDGE_LOOP ( 'NONE', ( #836, #9835, #17267, #1204 ) ) ;
#2776 = VECTOR ( 'NONE', #18591, 999.9999999999998863 ) ;
#2777 = CARTESIAN_POINT ( 'NONE',  ( 32.00000000000000000, 40.03620104880000241, -136.0552959530000123 ) ) ;
#2778 = LINE ( 'NONE', #8813, #4152 ) ;
#2779 = EDGE_LOOP ( 'NONE', ( #13040, #10289, #13027, #20220, #7821, #18203, #16899 ) ) ;
#2780 = FACE_OUTER_BOUND ( 'NONE', #8072, .T. ) ;
#2781 = ADVANCED_FACE ( 'NONE', ( #9182 ), #14563, .F. ) ;
#2782 = CARTESIAN_POINT ( 'NONE',  ( 20.50000000000000000, -20.50000000000000000, -150.0552959529999839 ) ) ;
#2783 = PLANE ( 'NONE',  #9361 ) ;
#2784 = DIRECTION ( 'NONE',  ( -8.956391184260000029E-12, 9.094947017729999296E-13, -1.000000000000000000 ) ) ;
#2785 = CARTESIAN_POINT ( 'NONE',  ( -10.46044647323697063, 34.41702787325856150, -147.4775189463319407 ) ) ;
#2786 = EDGE_CURVE ( 'NONE', #3754, #16830, #16459, .T. ) ;
#2787 = PLANE ( 'NONE',  #9299 ) ;
#2788 = CARTESIAN_POINT ( 'NONE',  ( -7.628878236750000319, 37.90286001179999431, -140.0026079769999683 ) ) ;
#2789 = VERTEX_POINT ( 'NONE', #3495 ) ;
#2790 =( NAMED_UNIT ( * ) SI_UNIT ( $, .STERADIAN. ) SOLID_ANGLE_UNIT ( ) );
#2791 = ORIENTED_EDGE ( 'NONE', *, *, #2440, .F. ) ;
#2792 = CARTESIAN_POINT ( 'NONE',  ( -7.305231917127300356, 34.61982510821351866, -147.5275647001010100 ) ) ;
#2793 = DIRECTION ( 'NONE',  ( 1.000000000000000000, 0.000000000000000000, 2.507771768019999718E-12 ) ) ;
#2794 = CARTESIAN_POINT ( 'NONE',  ( -20.45144833149999997, 36.94873838139999833, -139.8044047869999815 ) ) ;
#2795 = EDGE_LOOP ( 'NONE', ( #15530, #15621, #18074, #13138 ) ) ;
#2796 = CARTESIAN_POINT ( 'NONE',  ( -32.50000000000000000, 48.00000000000000000, -148.5552959529999839 ) ) ;
#2797 = DIRECTION ( 'NONE',  ( 1.000000000000000000, 2.602084704489999637E-17, -1.701177084830000066E-20 ) ) ;
#2798 = ORIENTED_EDGE ( 'NONE', *, *, #13125, .F. ) ;
#2799 = CARTESIAN_POINT ( 'NONE',  ( -21.02348081759773279, 37.67455232199478843, -147.5674820021630467 ) ) ;
#2800 = CARTESIAN_POINT ( 'NONE',  ( -17.89449017611291737, 39.21037955099460248, -147.0820833685213813 ) ) ;
#2801 = PRODUCT_DEFINITION_FORMATION_WITH_SPECIFIED_SOURCE ( 'ANY', '', #1896, .NOT_KNOWN. ) ;
#2802 = FACE_BOUND ( 'NONE', #7788, .T. ) ;
#2803 = FACE_OUTER_BOUND ( 'NONE', #950, .T. ) ;
#2804 = CARTESIAN_POINT ( 'NONE',  ( -25.71899619671468784, 33.84119088110737295, -142.2795079795113224 ) ) ;
#2805 = DIRECTION ( 'NONE',  ( 1.000000000000000000, 0.000000000000000000, -2.257453483404485235E-12 ) ) ;
#2806 = ADVANCED_FACE ( 'NONE', ( #9292 ), #16565, .T. ) ;
#2807 = ORIENTED_EDGE ( 'NONE', *, *, #8060, .T. ) ;
#2808 = DIRECTION ( 'NONE',  ( 0.000000000000000000, 0.000000000000000000, 1.000000000000000000 ) ) ;
#2809 = ORIENTED_EDGE ( 'NONE', *, *, #7368, .F. ) ;
#2810 = ORIENTED_EDGE ( 'NONE', *, *, #3283, .T. ) ;
#2811 = CARTESIAN_POINT ( 'NONE',  ( -38.72222222220000276, 29.00000000000000000, -140.5552959529999839 ) ) ;
#2812 = ADVANCED_FACE ( 'NONE', ( #10845 ), #5397, .T. ) ;
#2813 = VERTEX_POINT ( 'NONE', #7517 ) ;
#2814 = DIRECTION ( 'NONE',  ( 0.000000000000000000, 1.000000000000000000, 0.000000000000000000 ) ) ;
#2815 = ORIENTED_EDGE ( 'NONE', *, *, #21780, .F. ) ;
#2816 = ORIENTED_EDGE ( 'NONE', *, *, #14217, .T. ) ;
#2817 = CARTESIAN_POINT ( 'NONE',  ( 8.750000000000000000, -40.23606797749999942, -150.5552959529999839 ) ) ;
#2818 = CARTESIAN_POINT ( 'NONE',  ( -18.57919711151616582, 36.32393431488520719, -147.4152369972853762 ) ) ;
#2819 = DIRECTION ( 'NONE',  ( 0.000000000000000000, 6.069065783950000909E-29, -1.000000000000000000 ) ) ;
#2820 =( LENGTH_UNIT ( ) NAMED_UNIT ( * ) SI_UNIT ( .MILLI., .METRE. ) );
#2821 = SHAPE_REPRESENTATION ( 'Latch Return Spring', ( #5025 ), #3911 ) ;
#2822 = LINE ( 'NONE', #6734, #12933 ) ;
#2823 = ADVANCED_FACE ( 'NONE', ( #275 ), #7172, .F. ) ;
#2824 = LINE ( 'NONE', #22941, #17455 ) ;
#2825 = ORIENTED_EDGE ( 'NONE', *, *, #13893, .F. ) ;
#2826 = CARTESIAN_POINT ( 'NONE',  ( -27.47244207670000193, 35.09215423530000066, -148.2237751110000090 ) ) ;
#2827 = CARTESIAN_POINT ( 'NONE',  ( 9.629496873833184978, 37.99207690572956153, -146.3513483205671832 ) ) ;
#2828 = LINE ( 'NONE', #17456, #18607 ) ;
#2829 = EDGE_CURVE ( 'NONE', #17860, #14260, #14438, .T. ) ;
#2830 = ORIENTED_EDGE ( 'NONE', *, *, #8283, .T. ) ;
#2831 = CIRCLE ( 'NONE', #3974, 8.176568160360000448 ) ;
#2832 = LINE ( 'NONE', #23495, #17755 ) ;
#2833 = CARTESIAN_POINT ( 'NONE',  ( 3.999999999879999546, -5.500000000000000000, -135.4552959529999896 ) ) ;
#2834 = ORIENTED_EDGE ( 'NONE', *, *, #18308, .T. ) ;
#2835 = CARTESIAN_POINT ( 'NONE',  ( -33.42928932190000069, 15.47217712079999963, -141.3604938089999905 ) ) ;
#2836 = CARTESIAN_POINT ( 'NONE',  ( -4.499999999929999994, 42.50000000000000000, -138.0552959530000123 ) ) ;
#2837 = ORIENTED_EDGE ( 'NONE', *, *, #6869, .F. ) ;
#2838 = LINE ( 'NONE', #15334, #10249 ) ;
#2839 = CARTESIAN_POINT ( 'NONE',  ( 21.10099947280546218, -22.34364015992474961, -150.0552959529999839 ) ) ;
#2840 = ORIENTED_EDGE ( 'NONE', *, *, #4687, .T. ) ;
#2841 = CARTESIAN_POINT ( 'NONE',  ( -14.70419048427484121, 38.44039274178464893, -140.6418676086782682 ) ) ;
#2842 = EDGE_CURVE ( 'NONE', #17230, #13656, #10408, .T. ) ;
#2843 = LINE ( 'NONE', #17597, #14776 ) ;
#2844 = VERTEX_POINT ( 'NONE', #18013 ) ;
#2845 = EDGE_CURVE ( 'NONE', #22553, #22537, #13455, .T. ) ;
#2846 = CARTESIAN_POINT ( 'NONE',  ( 19.75551406279999966, -31.14090339520000228, -145.5552959529999839 ) ) ;
#2847 = ORIENTED_EDGE ( 'NONE', *, *, #10102, .T. ) ;
#2848 = DIRECTION ( 'NONE',  ( -0.7071067811865474617, 0.7071067811865476838, 0.000000000000000000 ) ) ;
#2849 = DIRECTION ( 'NONE',  ( 2.256861364460000137E-12, 0.000000000000000000, 1.000000000000000000 ) ) ;
#2850 = ORIENTED_EDGE ( 'NONE', *, *, #14751, .F. ) ;
#2851 = CARTESIAN_POINT ( 'NONE',  ( 0.000000000000000000, -36.00000000000000000, -150.0552959529999839 ) ) ;
#2852 = VERTEX_POINT ( 'NONE', #22052 ) ;
#2853 = EDGE_CURVE ( 'NONE', #19866, #13875, #5393, .T. ) ;
#2854 = DIRECTION ( 'NONE',  ( -1.000000000000000000, 0.000000000000000000, 2.257120985840000117E-12 ) ) ;
#2855 = EDGE_CURVE ( 'NONE', #21958, #6865, #16226, .T. ) ;
#2856 = LINE ( 'NONE', #3096, #10200 ) ;
#2857 = VECTOR ( 'NONE', #7846, 1000.000000000000000 ) ;
#2858 = ORIENTED_EDGE ( 'NONE', *, *, #5935, .T. ) ;
#2859 = EDGE_CURVE ( 'NONE', #5950, #5202, #2650, .T. ) ;
#2860 = EDGE_CURVE ( 'NONE', #17363, #12377, #2309, .T. ) ;
#2861 = ORIENTED_EDGE ( 'NONE', *, *, #11707, .F. ) ;
#2862 = LINE ( 'NONE', #8439, #13539 ) ;
#2863 = FACE_OUTER_BOUND ( 'NONE', #12833, .T. ) ;
#2864 = CARTESIAN_POINT ( 'NONE',  ( -20.60824191589999899, -32.00000000000000000, -150.0657682190000060 ) ) ;
#2865 = CARTESIAN_POINT ( 'NONE',  ( -9.434278515689999978, -18.41834002140000237, -146.5552959529999839 ) ) ;
#2866 = VERTEX_POINT ( 'NONE', #749 ) ;
#2867 = CARTESIAN_POINT ( 'NONE',  ( 4.999999999879999990, -3.500000000000000000, -132.9059375850000038 ) ) ;
#2868 = CARTESIAN_POINT ( 'NONE',  ( -22.10824191589999899, -34.50000000000000000, -146.3157682190000060 ) ) ;
#2869 = DIRECTION ( 'NONE',  ( 3.882490197650000213E-51, -1.000000000000000000, -4.009147065150000317E-51 ) ) ;
#2870 = CARTESIAN_POINT ( 'NONE',  ( -14.24276452920772051, -41.69048151115483591, -150.0552959529999839 ) ) ;
#2871 = CARTESIAN_POINT ( 'NONE',  ( 16.65421564080000039, -18.61497348660000029, -145.5552959529999839 ) ) ;
#2872 = LINE ( 'NONE', #6434, #2995 ) ;
#2873 = VECTOR ( 'NONE', #6427, 1000.000000000000000 ) ;
#2874 = AXIS2_PLACEMENT_3D ( 'NONE', #16722, #23523, #18291 ) ;
#2875 = ORIENTED_EDGE ( 'NONE', *, *, #22649, .F. ) ;
#2876 = CARTESIAN_POINT ( 'NONE',  ( -9.363082409902974135, -24.97989489974943567, -147.5552959529923953 ) ) ;
#2877 = LINE ( 'NONE', #3000, #6429 ) ;
#2878 = CARTESIAN_POINT ( 'NONE',  ( -4.683324139160000676, 37.83302525630000446, -140.3020749749999823 ) ) ;
#2879 = DIRECTION ( 'NONE',  ( 8.954614827420000395E-12, -9.094947017729999296E-13, 1.000000000000000000 ) ) ;
#2880 = B_SPLINE_CURVE_WITH_KNOTS ( 'NONE', 3,
 ( #9732, #11287, #9621, #6297, #18691, #20594, #7729, #371, #22605, #16780 ),
 .UNSPECIFIED., .F., .F.,
 ( 4, 2, 2, 2, 4 ),
 ( 0.000000000000000000, 0.2500000000000000000, 0.5000000000000000000, 0.7500000000000000000, 1.000000000000000000 ),
 .UNSPECIFIED. ) ;
#2881 = DIRECTION ( 'NONE',  ( 1.000000000000000000, 0.000000000000000000, -2.262368070660000099E-12 ) ) ;
#2882 = ORIENTED_EDGE ( 'NONE', *, *, #4143, .F. ) ;
#2883 = CARTESIAN_POINT ( 'NONE',  ( -9.834719431799998191, 32.58365614919999587, -144.2353630830000100 ) ) ;
#2884 = DIRECTION ( 'NONE',  ( 0.000000000000000000, 1.000000000000000000, 0.000000000000000000 ) ) ;
#2885 = EDGE_CURVE ( 'NONE', #546, #14999, #14216, .T. ) ;
#2886 = DIRECTION ( 'NONE',  ( 0.000000000000000000, -1.000000000000000000, -2.341876234024414612E-17 ) ) ;
#2887 = EDGE_LOOP ( 'NONE', ( #19953, #13891, #13269, #16498 ) ) ;
#2888 = PRODUCT_DEFINITION_SHAPE ( 'NONE', 'NONE',  #23542 ) ;
#2889 = DIRECTION ( 'NONE',  ( 5.094701932209999624E-24, 1.000000000000000000, 0.000000000000000000 ) ) ;
#2891 = LINE ( 'NONE', #2777, #9448 ) ;
#2890 = VECTOR ( 'NONE', #17226, 1000.000000000000000 ) ;
#2892 = AXIS2_PLACEMENT_3D ( 'NONE', #9069, #7528, #21838 ) ;
#2893 = CARTESIAN_POINT ( 'NONE',  ( -12.50000000000000000, 0.000000000000000000, -150.0552959529999839 ) ) ;
#2894 = VERTEX_POINT ( 'NONE', #7863 ) ;
#2895 = DIRECTION ( 'NONE',  ( 0.000000000000000000, 0.000000000000000000, 1.000000000000000000 ) ) ;
#2896 = CARTESIAN_POINT ( 'NONE',  ( 16.33424841169999908, -31.58611763329999889, -148.5552959529999839 ) ) ;
#2897 = CARTESIAN_POINT ( 'NONE',  ( -0.009529796614447350739, 16.74243713058418237, -150.0552959529999839 ) ) ;
#2898 = CARTESIAN_POINT ( 'NONE',  ( -34.47299999999999898, 15.75516512379999945, -143.0964448760000209 ) ) ;
#2899 = CARTESIAN_POINT ( 'NONE',  ( -10.88223456478890938, 32.81667835592666904, -144.3412242124914258 ) ) ;
#2900 = CARTESIAN_POINT ( 'NONE',  ( 5.519240656394276634, 27.95201674008764314, -150.0552959530000123 ) ) ;
#2901 = CARTESIAN_POINT ( 'NONE',  ( 5.569521322412388287, -33.22557888555225247, -150.0552959530000123 ) ) ;
#2902 = ORIENTED_EDGE ( 'NONE', *, *, #9008, .F. ) ;
#2903 = CARTESIAN_POINT ( 'NONE',  ( -20.93854596064992180, 37.74500530009579791, -147.9603137871160072 ) ) ;
#2904 = FILL_AREA_STYLE_COLOUR ( '', #22146 ) ;
#2905 = ORIENTED_EDGE ( 'NONE', *, *, #3505, .T. ) ;
#2906 = AXIS2_PLACEMENT_3D ( 'NONE', #23201, #23316, #21540 ) ;
#2907 = CARTESIAN_POINT ( 'NONE',  ( -7.987711783864115844, 33.66592685080672709, -142.2820551195727319 ) ) ;
#2908 = CARTESIAN_POINT ( 'NONE',  ( -29.86462848809999926, 41.46897301219999576, -145.0541174280000121 ) ) ;
#2909 = VECTOR ( 'NONE', #15147, 1000.000000000000000 ) ;
#2910 = CARTESIAN_POINT ( 'NONE',  ( -21.29590688489999906, 41.28591597809999314, -144.5271551099999954 ) ) ;
#2911 = ORIENTED_EDGE ( 'NONE', *, *, #4437, .T. ) ;
#2912 = EDGE_CURVE ( 'NONE', #1217, #4350, #11196, .T. ) ;
#2913 = CARTESIAN_POINT ( 'NONE',  ( 8.500000000050000892, 37.00000000000000000, -146.5552959529999839 ) ) ;
#2914 = LINE ( 'NONE', #1366, #9859 ) ;
#2915 = ORIENTED_EDGE ( 'NONE', *, *, #2220, .T. ) ;
#2916 = PLANE ( 'NONE',  #19017 ) ;
#2917 = CARTESIAN_POINT ( 'NONE',  ( -17.98362287481939248, 39.30401989832888177, -140.6846516121062223 ) ) ;
#2918 = DIRECTION ( 'NONE',  ( 1.000000000000000000, 0.000000000000000000, 0.000000000000000000 ) ) ;
#2919 = CARTESIAN_POINT ( 'NONE',  ( 6.999993628236942378, 36.89957845934668512, -146.5552973561658803 ) ) ;
#2920 = CARTESIAN_POINT ( 'NONE',  ( -31.00000000000000000, 19.50000000000000000, -150.5552959529999839 ) ) ;
#2921 = VECTOR ( 'NONE', #13977, 1000.000000000000000 ) ;
#2922 = CARTESIAN_POINT ( 'NONE',  ( -24.58801263762544309, 32.96925759728824090, -144.4410906680583082 ) ) ;
#2923 = CARTESIAN_POINT ( 'NONE',  ( -32.50000000000000000, 21.50000000000000000, -137.0552959530000123 ) ) ;
#2924 = CARTESIAN_POINT ( 'NONE',  ( -12.46649926358460725, 41.37859836428589944, -144.5903357203852124 ) ) ;
#2925 = EDGE_LOOP ( 'NONE', ( #21956, #13989, #16727, #2445 ) ) ;
#2926 = CARTESIAN_POINT ( 'NONE',  ( 4.499999999879999102, -3.500000000000000000, -136.0552959530000123 ) ) ;
#2927 = EDGE_LOOP ( 'NONE', ( #19202, #2312, #18251, #1135, #8034 ) ) ;
#2928 = CARTESIAN_POINT ( 'NONE',  ( 19.68320006079999729, -24.50000000000000000, -150.0552959529999839 ) ) ;
#2929 = VERTEX_POINT ( 'NONE', #13108 ) ;
#2930 = DIRECTION ( 'NONE',  ( 1.000000000000000000, 0.000000000000000000, 0.000000000000000000 ) ) ;
#2931 = ORIENTED_EDGE ( 'NONE', *, *, #4863, .F. ) ;
#2932 = CARTESIAN_POINT ( 'NONE',  ( 1.544832289376347534, 26.15117705467465115, -136.0552959530034798 ) ) ;
#2933 = VERTEX_POINT ( 'NONE', #628 ) ;
#2934 = AXIS2_PLACEMENT_3D ( 'NONE', #2198, #7420, #5865 ) ;
#2935 = VERTEX_POINT ( 'NONE', #22164 ) ;
#2936 = EDGE_CURVE ( 'NONE', #6697, #963, #5850, .T. ) ;
#2937 = DIRECTION ( 'NONE',  ( 1.000000000000000000, 2.602084704489999637E-17, -1.701177084980000217E-20 ) ) ;
#2938 = CARTESIAN_POINT ( 'NONE',  ( -18.46643761660000038, 34.84883242739999787, -147.1252693400000169 ) ) ;
#2939 = AXIS2_PLACEMENT_3D ( 'NONE', #9169, #5385, #3358 ) ;
#2940 = DIRECTION ( 'NONE',  ( 1.000000000000000000, 2.602084704489999637E-17, 0.000000000000000000 ) ) ;
#2941 = EDGE_CURVE ( 'NONE', #1936, #19224, #9535, .T. ) ;
#2942 = CARTESIAN_POINT ( 'NONE',  ( -21.55459145674873866, -3.250000000000984102, -146.3157682189986133 ) ) ;
#2943 = CARTESIAN_POINT ( 'NONE',  ( -7.015833805750000707, 33.30032478630000270, -141.9582197170000200 ) ) ;
#2944 = CARTESIAN_POINT ( 'NONE',  ( -9.410060017898935314, 41.36342684009822079, -144.4162120660980122 ) ) ;
#2945 = ORIENTED_EDGE ( 'NONE', *, *, #17078, .T. ) ;
#2946 = CARTESIAN_POINT ( 'NONE',  ( -28.37825339579999806, 32.94869610819999650, -141.6352474660000098 ) ) ;
#2947 = CARTESIAN_POINT ( 'NONE',  ( 9.125765718317245145, 38.36348339572941057, -146.1507818850132026 ) ) ;
#2948 = CARTESIAN_POINT ( 'NONE',  ( -4.500000000000000000, 37.00000000000000000, -151.0552959529999839 ) ) ;
#2949 = VERTEX_POINT ( 'NONE', #11435 ) ;
#2950 = VECTOR ( 'NONE', #13412, 999.9999999999998863 ) ;
#2951 = CARTESIAN_POINT ( 'NONE',  ( 1.847645635000000119, -15.93876195360000025, -146.5552959529999839 ) ) ;
#2952 = FACE_OUTER_BOUND ( 'NONE', #9670, .T. ) ;
#2953 = VECTOR ( 'NONE', #4150, 1000.000000000000114 ) ;
#2954 = ORIENTED_EDGE ( 'NONE', *, *, #12303, .T. ) ;
#2955 = CARTESIAN_POINT ( 'NONE',  ( -32.50000000000000000, -35.00000000000000000, -145.5552959529999839 ) ) ;
#2956 = CARTESIAN_POINT ( 'NONE',  ( 19.91945158500000090, -51.14507942810000429, -149.5552959529999839 ) ) ;
#2957 = EDGE_CURVE ( 'NONE', #1286, #6185, #20380, .T. ) ;
#2958 = ORIENTED_EDGE ( 'NONE', *, *, #497, .T. ) ;
#2959 = CARTESIAN_POINT ( 'NONE',  ( -18.07392865170000107, -18.00000000000000000, -147.3157682190000060 ) ) ;
#2960 = CARTESIAN_POINT ( 'NONE',  ( -18.31895680040000229, 41.06933176500000116, -146.2870363079999834 ) ) ;
#2961 = EDGE_LOOP ( 'NONE', ( #20948, #1183, #3454, #23267 ) ) ;
#2962 = CARTESIAN_POINT ( 'NONE',  ( 6.500000000000000000, 13.00000000000000000, -150.5552959529999839 ) ) ;
#2963 = APPLICATION_CONTEXT ( 'automotive_design' ) ;
#2964 = CARTESIAN_POINT ( 'NONE',  ( -26.30700737260927369, 34.29719532912928059, -140.4927034919771245 ) ) ;
#2965 = ORIENTED_EDGE ( 'NONE', *, *, #20292, .F. ) ;
#2966 = SURFACE_STYLE_USAGE ( .BOTH. , #6176 ) ;
#2967 =( BOUNDED_SURFACE ( )  B_SPLINE_SURFACE ( 5, 5, ( 
 ( #5332, #10779, #5093, #21521, #19962, #10428 ),
 ( #3664, #23181, #1775, #8641, #16279, #17706 ),
 ( #17825, #1893, #6874, #9116, #7348, #14142 ),
 ( #3307, #23535, #108, #1542, #8764, #6995 ),
 ( #5203, #14953, #9580, #18301, #13047, #12808 ),
 ( #11359, #4246, #2234, #7567, #20318, #18759 ),
 ( #9691, #12927, #678, #4012, #3902, #22214 ),
 ( #3781, #11241, #16966, #14842, #9454, #18513 ),
 ( #20082, #7797, #11023, #11481, #2117, #16733 ),
 ( #22101, #2470, #7910, #2015, #21876, #2359 ),
 ( #20207, #447, #5560, #18641, #9235, #16502 ),
 ( #208, #20426, #7684, #16854, #11133, #7452 ) ),
 .UNSPECIFIED., .F., .F., .F. ) 
 B_SPLINE_SURFACE_WITH_KNOTS ( ( 6, 3, 3, 6 ),
 ( 6, 6 ),
 ( 0.000000000000000000, 4.463483057499999518, 8.880954762089999122, 13.25426345570000031 ),
 ( 0.000000000000000000, 1.570796326817224919 ),
 .UNSPECIFIED. ) 
 GEOMETRIC_REPRESENTATION_ITEM ( )  RATIONAL_B_SPLINE_SURFACE ( (
 ( 1.000000000000000000, 0.5999999999943410600, 0.3999999999943409934, 0.2999999999957554953, 0.2499999999971705134, 0.2500000000000000000),
 ( 1.000000000000000000, 0.5999999999943410600, 0.3999999999943409934, 0.2999999999957554953, 0.2499999999971705134, 0.2500000000000000000),
 ( 1.000000000000000000, 0.5999999999943410600, 0.3999999999943409934, 0.2999999999957554953, 0.2499999999971705134, 0.2500000000000000000),
 ( 1.000000000000000000, 0.5999999999943410600, 0.3999999999943409934, 0.2999999999957554953, 0.2499999999971705134, 0.2500000000000000000),
 ( 1.000000000000000000, 0.5999999999943410600, 0.3999999999943409934, 0.2999999999957554953, 0.2499999999971705134, 0.2500000000000000000),
 ( 1.000000000000000000, 0.5999999999943410600, 0.3999999999943409934, 0.2999999999957554953, 0.2499999999971705134, 0.2500000000000000000),
 ( 1.000000000000000000, 0.5999999999943410600, 0.3999999999943409934, 0.2999999999957554953, 0.2499999999971705134, 0.2500000000000000000),
 ( 1.000000000000000000, 0.5999999999943410600, 0.3999999999943409934, 0.2999999999957554953, 0.2499999999971705134, 0.2500000000000000000),
 ( 1.000000000000000000, 0.5999999999943410600, 0.3999999999943409934, 0.2999999999957554953, 0.2499999999971705134, 0.2500000000000000000),
 ( 1.000000000000000000, 0.5999999999943410600, 0.3999999999943409934, 0.2999999999957554953, 0.2499999999971705134, 0.2500000000000000000),
 ( 1.000000000000000000, 0.5999999999943410600, 0.3999999999943409934, 0.2999999999957554953, 0.2499999999971705134, 0.2500000000000000000),
 ( 1.000000000000000000, 0.5999999999943410600, 0.3999999999943409934, 0.2999999999957554953, 0.2499999999971705134, 0.2500000000000000000) ) ) 
 REPRESENTATION_ITEM ( '' )  SURFACE ( )  );
#2968 = LINE ( 'NONE', #15450, #2688 ) ;
#2969 = ORIENTED_EDGE ( 'NONE', *, *, #11432, .T. ) ;
#2970 = CARTESIAN_POINT ( 'NONE',  ( -12.04808041669999952, 40.71874701600000179, -143.7411651109999866 ) ) ;
#2971 = DIRECTION ( 'NONE',  ( 0.000000000000000000, 0.000000000000000000, -1.000000000000000000 ) ) ;
#2972 = EDGE_LOOP ( 'NONE', ( #3946, #14498, #19451, #3090 ) ) ;
#2973 = ADVANCED_FACE ( 'NONE', ( #6094 ), #18718, .T. ) ;
#2974 = CARTESIAN_POINT ( 'NONE',  ( -34.50000000000000000, 67.50000000000000000, -144.0552959529999839 ) ) ;
#2975 = VECTOR ( 'NONE', #13953, 1000.000000000000000 ) ;
#2976 = PLANE ( 'NONE',  #18950 ) ;
#2977 = CIRCLE ( 'NONE', #16272, 1.499999999999999556 ) ;
#2978 = DIRECTION ( 'NONE',  ( -0.1270149847699686696, -0.9919007982877545704, 8.287421350277954308E-13 ) ) ;
#2979 = EDGE_CURVE ( 'NONE', #9664, #21739, #2426, .T. ) ;
#2980 = VERTEX_POINT ( 'NONE', #4420 ) ;
#2981 = CARTESIAN_POINT ( 'NONE',  ( 4.892699081698721919, -0.4999999999999995559, -150.0552959529999839 ) ) ;
#2982 = DIRECTION ( 'NONE',  ( -0.9953753789357124848, 0.09606172499277225441, 7.355811845627876534E-14 ) ) ;
#2983 = CARTESIAN_POINT ( 'NONE',  ( -14.06829009843223766, 40.90462708772086842, -143.6915823990867409 ) ) ;
#2984 = DIRECTION ( 'NONE',  ( 0.000000000000000000, 1.000000000000000000, 0.000000000000000000 ) ) ;
#2985 = ORIENTED_EDGE ( 'NONE', *, *, #5466, .T. ) ;
#2986 = DIRECTION ( 'NONE',  ( 1.211690350419999855E-27, 2.765629237170000203E-27, -1.000000000000000000 ) ) ;
#2987 = CARTESIAN_POINT ( 'NONE',  ( -32.50000000000000000, 21.50000000000000000, -136.0552959530000123 ) ) ;
#2988 = VECTOR ( 'NONE', #6917, 1000.000000000000000 ) ;
#2989 = EDGE_CURVE ( 'NONE', #7959, #22754, #17153, .T. ) ;
#2990 = CARTESIAN_POINT ( 'NONE',  ( 25.34364015992474961, -18.10099947280545862, -150.0552959529999839 ) ) ;
#2991 = CARTESIAN_POINT ( 'NONE',  ( 5.347956485829999274, -22.34165470570000167, -146.5552959529999839 ) ) ;
#2992 = DIRECTION ( 'NONE',  ( -2.507771768019999718E-12, -1.592654864069999939E-17, 1.000000000000000000 ) ) ;
#2993 = DIRECTION ( 'NONE',  ( 1.526468026909999897E-13, 8.159623473500000156E-13, 1.000000000000000000 ) ) ;
#2994 = EDGE_CURVE ( 'NONE', #4187, #11995, #12996, .T. ) ;
#2995 = VECTOR ( 'NONE', #22865, 1000.000000000000000 ) ;
#2996 = ORIENTED_EDGE ( 'NONE', *, *, #17303, .T. ) ;
#2997 = DIRECTION ( 'NONE',  ( -1.000000000000000000, 5.094701932209999624E-24, 0.000000000000000000 ) ) ;
#2998 = ADVANCED_FACE ( 'NONE', ( #20270 ), #4074, .F. ) ;
#2999 = VECTOR ( 'NONE', #17361, 1000.000000000000000 ) ;
#3000 = CARTESIAN_POINT ( 'NONE',  ( 5.631397321050000571, -17.85059010000000157, -147.5552959529999839 ) ) ;
#3001 = EDGE_CURVE ( 'NONE', #23414, #20938, #18469, .T. ) ;
#3002 = LINE ( 'NONE', #6438, #21364 ) ;
#3003 = CARTESIAN_POINT ( 'NONE',  ( -7.129475577410000042, -25.57825421080000083, -144.5552959529999839 ) ) ;
#3004 = DIRECTION ( 'NONE',  ( 0.000000000000000000, 0.000000000000000000, 1.000000000000000000 ) ) ;
#3005 = ORIENTED_EDGE ( 'NONE', *, *, #4849, .F. ) ;
#3006 = CARTESIAN_POINT ( 'NONE',  ( 23.17093239529999948, -15.44501179329999907, -144.0552959529999839 ) ) ;
#3007 = PLANE ( 'NONE',  #19489 ) ;
#3008 = DIRECTION ( 'NONE',  ( 1.000000000000000000, 0.000000000000000000, 0.000000000000000000 ) ) ;
#3009 = ORIENTED_EDGE ( 'NONE', *, *, #12709, .F. ) ;
#3010 = CARTESIAN_POINT ( 'NONE',  ( -30.99999999989999822, 47.50000000000000000, -138.5552959529999839 ) ) ;
#3011 = VECTOR ( 'NONE', #19976, 1000.000000000000000 ) ;
#3012 = VECTOR ( 'NONE', #2784, 1000.000000000000000 ) ;
#3013 = CARTESIAN_POINT ( 'NONE',  ( -29.19447537614601274, 33.38066814340002963, -141.9968987688876609 ) ) ;
#3014 = CARTESIAN_POINT ( 'NONE',  ( 5.749999999879999102, -3.000000000000000000, -135.0552959530000123 ) ) ;
#3015 = ORIENTED_EDGE ( 'NONE', *, *, #10411, .T. ) ;
#3016 = AXIS2_PLACEMENT_3D ( 'NONE', #9727, #4167, #17003 ) ;
#3017 = CARTESIAN_POINT ( 'NONE',  ( -23.66625742371592978, 40.06790428317820130, -142.3133758147152435 ) ) ;
#3018 = CARTESIAN_POINT ( 'NONE',  ( 2.500000000170000014, 24.50000000000000000, -136.5552959530000123 ) ) ;
#3019 = AXIS2_PLACEMENT_3D ( 'NONE', #13523, #15082, #17336 ) ;
#3020 = CARTESIAN_POINT ( 'NONE',  ( -15.00000000000000000, -43.00000000000000000, -140.0552959529999839 ) ) ;
#3021 = CARTESIAN_POINT ( 'NONE',  ( -12.50000000000000000, 45.50000000000000000, -137.0552959530000123 ) ) ;
#3022 = VERTEX_POINT ( 'NONE', #18586 ) ;
#3023 = CARTESIAN_POINT ( 'NONE',  ( -4.875412749849999727, 39.32116320210000282, -140.9191069839999955 ) ) ;
#3024 = PLANE ( 'NONE',  #11971 ) ;
#3025 = EDGE_CURVE ( 'NONE', #6070, #18790, #397, .T. ) ;
#3026 = CARTESIAN_POINT ( 'NONE',  ( 5.298801200312091453, -33.35703351611178391, -150.0552959530000123 ) ) ;
#3027 = LINE ( 'NONE', #3142, #3483 ) ;
#3028 = ORIENTED_EDGE ( 'NONE', *, *, #20273, .F. ) ;
#3029 = EDGE_CURVE ( 'NONE', #1422, #22304, #7634, .T. ) ;
#3030 = AXIS2_PLACEMENT_3D ( 'NONE', #3237, #21215, #10587 ) ;
#3031 = VECTOR ( 'NONE', #3216, 999.9999999999998863 ) ;
#3032 = ORIENTED_EDGE ( 'NONE', *, *, #18308, .F. ) ;
#3033 = CARTESIAN_POINT ( 'NONE',  ( -7.384580498943978277, 36.26220355060780065, -140.3078533517004303 ) ) ;
#3034 = CARTESIAN_POINT ( 'NONE',  ( 6.830232017748067541, -28.71493780969095511, -144.5552959530278656 ) ) ;
#3035 = CARTESIAN_POINT ( 'NONE',  ( 25.96278831570000278, 46.03148680969999873, -136.0552959530000123 ) ) ;
#3036 = AXIS2_PLACEMENT_3D ( 'NONE', #17242, #14148, #8427 ) ;
#3037 = VERTEX_POINT ( 'NONE', #2532 ) ;
#3038 = CARTESIAN_POINT ( 'NONE',  ( 32.50000000000000000, 20.96379895120000114, -136.0552959530000123 ) ) ;
#3039 = CARTESIAN_POINT ( 'NONE',  ( -14.12781175210000129, 38.88127384660000274, -139.8125553750000165 ) ) ;
#3040 = VERTEX_POINT ( 'NONE', #7750 ) ;
#3041 = LINE ( 'NONE', #22661, #12557 ) ;
#3042 = CARTESIAN_POINT ( 'NONE',  ( -17.52779041587893971, 36.93962571632589231, -139.7364823516947467 ) ) ;
#3043 = LINE ( 'NONE', #22910, #10486 ) ;
#3044 = CARTESIAN_POINT ( 'NONE',  ( -12.94305406498006761, 37.05025962682653784, -148.5780888799760078 ) ) ;
#3045 = AXIS2_PLACEMENT_3D ( 'NONE', #3653, #21396, #10418 ) ;
#3046 = DIRECTION ( 'NONE',  ( 0.000000000000000000, 1.000000000000000000, 0.000000000000000000 ) ) ;
#3047 = CARTESIAN_POINT ( 'NONE',  ( -24.78493530337882333, 34.98244403198583541, -146.8404575437234314 ) ) ;
#3048 = CARTESIAN_POINT ( 'NONE',  ( 10.38320006080000013, -24.50000000000000000, -149.3052959529999839 ) ) ;
#3049 = AXIS2_PLACEMENT_3D ( 'NONE', #5771, #2339, #4341 ) ;
#3050 = DIRECTION ( 'NONE',  ( -1.000000000000000000, 2.312964634635743450E-15, 0.000000000000000000 ) ) ;
#3051 = VECTOR ( 'NONE', #8892, 1000.000000000000000 ) ;
#3052 = EDGE_CURVE ( 'NONE', #20700, #18344, #20497, .T. ) ;
#3053 = AXIS2_PLACEMENT_3D ( 'NONE', #16643, #5930, #3928 ) ;
#3054 = VECTOR ( 'NONE', #12463, 999.9999999999998863 ) ;
#3055 = ORIENTED_EDGE ( 'NONE', *, *, #14144, .F. ) ;
#3056 = DIRECTION ( 'NONE',  ( -2.257157423930000049E-12, 0.000000000000000000, -1.000000000000000000 ) ) ;
#3057 = UNCERTAINTY_MEASURE_WITH_UNIT (LENGTH_MEASURE( 1.000000000000000082E-05 ), #7536, 'distance_accuracy_value', 'NONE');
#3058 = ORIENTED_EDGE ( 'NONE', *, *, #3585, .F. ) ;
#3059 = EDGE_LOOP ( 'NONE', ( #561, #7030, #15212, #3298, #21693, #7616 ) ) ;
#3060 = ORIENTED_EDGE ( 'NONE', *, *, #6740, .F. ) ;
#3061 = DIRECTION ( 'NONE',  ( -1.000000000000000000, 5.094701932209999624E-24, 2.257144641399999941E-12 ) ) ;
#3062 = CARTESIAN_POINT ( 'NONE',  ( 4.374398326270000581, -26.09174856970000178, -143.5552959529999839 ) ) ;
#3063 = ORIENTED_EDGE ( 'NONE', *, *, #19396, .T. ) ;
#3064 = ORIENTED_EDGE ( 'NONE', *, *, #19556, .T. ) ;
#3065 = CARTESIAN_POINT ( 'NONE',  ( -6.603585321229999749, -20.59801339440000234, -143.5552959529999839 ) ) ;
#3066 = CARTESIAN_POINT ( 'NONE',  ( -15.46613156839999981, 36.99333119719999985, -147.5584717940000132 ) ) ;
#3067 = SURFACE_STYLE_USAGE ( .BOTH. , #1172 ) ;
#3068 = VECTOR ( 'NONE', #2276, 1000.000000000000114 ) ;
#3069 = CARTESIAN_POINT ( 'NONE',  ( -8.462924335808684972, 36.00512048834733037, -139.7368446338785191 ) ) ;
#3070 = CARTESIAN_POINT ( 'NONE',  ( -9.292483939522659497, 40.96918990745680134, -144.3907905727278091 ) ) ;
#3071 = ORIENTED_EDGE ( 'NONE', *, *, #13452, .T. ) ;
#3072 = CARTESIAN_POINT ( 'NONE',  ( 3.611688725869999975E-11, 48.50000000000000000, -136.0552959530000123 ) ) ;
#3073 = DIRECTION ( 'NONE',  ( 0.000000000000000000, 1.000000000000000000, 0.000000000000000000 ) ) ;
#3074 = CARTESIAN_POINT ( 'NONE',  ( 25.42349012524837093, 35.71905350741751306, -150.0552959529999839 ) ) ;
#3075 = VERTEX_POINT ( 'NONE', #16916 ) ;
#3076 = EDGE_CURVE ( 'NONE', #12377, #11046, #9755, .T. ) ;
#3077 = FACE_OUTER_BOUND ( 'NONE', #8007, .T. ) ;
#3078 = ORIENTED_EDGE ( 'NONE', *, *, #9382, .T. ) ;
#3079 = LINE ( 'NONE', #8166, #15110 ) ;
#3080 = EDGE_CURVE ( 'NONE', #11246, #20820, #12262, .T. ) ;
#3081 = DIRECTION ( 'NONE',  ( 1.000000000000000000, 0.000000000000000000, 0.000000000000000000 ) ) ;
#3082 = VECTOR ( 'NONE', #6468, 1000.000000000000000 ) ;
#3083 = ORIENTED_EDGE ( 'NONE', *, *, #7044, .T. ) ;
#3084 = CARTESIAN_POINT ( 'NONE',  ( -22.52780672249999938, 37.05898997719999954, -140.0074087190000114 ) ) ;
#3085 = FACE_OUTER_BOUND ( 'NONE', #9259, .T. ) ;
#3086 = ORIENTED_EDGE ( 'NONE', *, *, #14144, .T. ) ;
#3087 = CARTESIAN_POINT ( 'NONE',  ( -14.21887350771891967, 37.71951061620244161, -140.5431489171321857 ) ) ;
#3088 = CARTESIAN_POINT ( 'NONE',  ( -26.39607007120000048, 36.95534867429999792, -140.3840478969999879 ) ) ;
#3089 = ORIENTED_EDGE ( 'NONE', *, *, #3888, .T. ) ;
#3090 = ORIENTED_EDGE ( 'NONE', *, *, #2989, .F. ) ;
#3091 = CARTESIAN_POINT ( 'NONE',  ( -12.66714788130000002, 37.75265353620000042, -147.6129237410000030 ) ) ;
#3092 = DIRECTION ( 'NONE',  ( 1.000000000000000000, 0.000000000000000000, -2.257171095940000041E-12 ) ) ;
#3093 = EDGE_LOOP ( 'NONE', ( #12559, #10314, #22259, #7596 ) ) ;
#3094 = CARTESIAN_POINT ( 'NONE',  ( -21.35824191589185972, -32.00000000000000000, -149.4708568729758724 ) ) ;
#3095 = FACE_OUTER_BOUND ( 'NONE', #7603, .T. ) ;
#3096 = CARTESIAN_POINT ( 'NONE',  ( 25.94418247360000152, 46.04723021459999899, -149.5552959529999839 ) ) ;
#3097 = AXIS2_PLACEMENT_3D ( 'NONE', #14363, #8756, #16035 ) ;
#3098 = VECTOR ( 'NONE', #14342, 1000.000000000000000 ) ;
#3099 = VECTOR ( 'NONE', #12871, 1000.000000000000227 ) ;
#3100 = ORIENTED_EDGE ( 'NONE', *, *, #5461, .F. ) ;
#3101 = DIRECTION ( 'NONE',  ( 0.6459422414661292189, -0.7633862853691524286, 2.257144641400451094E-12 ) ) ;
#3102 = FACE_OUTER_BOUND ( 'NONE', #4595, .T. ) ;
#3103 = CARTESIAN_POINT ( 'NONE',  ( -14.62351239453423091, 39.57503987224152553, -147.6848723493663726 ) ) ;
#3104 = CARTESIAN_POINT ( 'NONE',  ( -28.52142019844505327, 37.05975231236403999, -139.6605181375938685 ) ) ;
#3105 = ORIENTED_EDGE ( 'NONE', *, *, #4201, .F. ) ;
#3106 = DIRECTION ( 'NONE',  ( 0.000000000000000000, 1.000000000000000000, 0.000000000000000000 ) ) ;
#3107 = EDGE_CURVE ( 'NONE', #11140, #10546, #15835, .T. ) ;
#3108 = LINE ( 'NONE', #8550, #3259 ) ;
#3109 =( BOUNDED_CURVE ( )  B_SPLINE_CURVE ( 5, ( #1415, #6636, #19610, #14012, #21284, #17467 ),
 .UNSPECIFIED., .F., .F. ) 
 B_SPLINE_CURVE_WITH_KNOTS ( ( 6, 6 ),
 ( 0.000000000000000000, 1.570796326526077813 ),
 .UNSPECIFIED. ) 
 CURVE ( )  GEOMETRIC_REPRESENTATION_ITEM ( )  RATIONAL_B_SPLINE_CURVE ( ( 1.000000000000000000, 0.6000000000684805324, 0.4000000000684805213, 0.3000000000513604048, 0.2500000000342402773, 0.2500000000000000555 ) ) 
 REPRESENTATION_ITEM ( '' )  );
#3110 = CARTESIAN_POINT ( 'NONE',  ( 26.12135916506276345, -18.98914305888729714, -150.0552959530000123 ) ) ;
#3111 = PLANE ( 'NONE',  #18615 ) ;
#3112 = DIRECTION ( 'NONE',  ( 0.000000000000000000, -1.000000000000000000, 0.000000000000000000 ) ) ;
#3113 = DIRECTION ( 'NONE',  ( -0.6689647316207345540, 0.000000000000000000, 0.7432941462487100415 ) ) ;
#3114 = AXIS2_PLACEMENT_3D ( 'NONE', #12481, #19993, #14399 ) ;
#3115 = VERTEX_POINT ( 'NONE', #8563 ) ;
#3116 = AXIS2_PLACEMENT_3D ( 'NONE', #15395, #10140, #10272 ) ;
#3117 = CIRCLE ( 'NONE', #19457, 1.500000000000000444 ) ;
#3118 = CARTESIAN_POINT ( 'NONE',  ( -16.36311878257998842, 35.26028592910842008, -139.7765051114957089 ) ) ;
#3119 = CARTESIAN_POINT ( 'NONE',  ( -31.00000000000000000, -50.00000000000000000, -151.0552959529999839 ) ) ;
#3120 = ADVANCED_FACE ( 'NONE', ( #13826 ), #3123, .F. ) ;
#3121 = CARTESIAN_POINT ( 'NONE',  ( 12.50000000020000002, 24.10555127549999810, -136.5552959530000123 ) ) ;
#3122 = CARTESIAN_POINT ( 'NONE',  ( -24.78261485200000180, 38.62237172060000034, -147.6366313890000015 ) ) ;
#3123 = PLANE ( 'NONE',  #22201 ) ;
#3124 = VERTEX_POINT ( 'NONE', #19059 ) ;
#3125 = DIRECTION ( 'NONE',  ( -2.257144641399999941E-12, 0.000000000000000000, 1.000000000000000000 ) ) ;
#3126 = DIRECTION ( 'NONE',  ( 2.257157423930000049E-12, 0.000000000000000000, 1.000000000000000000 ) ) ;
#3127 = ORIENTED_EDGE ( 'NONE', *, *, #10459, .F. ) ;
#3128 = EDGE_CURVE ( 'NONE', #11242, #23163, #18023, .T. ) ;
#3129 = CARTESIAN_POINT ( 'NONE',  ( -29.35976486581876799, 36.20619751666908570, -140.4758582103364120 ) ) ;
#3130 = CARTESIAN_POINT ( 'NONE',  ( -4.499999999959999109, 40.00000000000000000, -153.0552959529999839 ) ) ;
#3131 = ORIENTED_EDGE ( 'NONE', *, *, #1335, .T. ) ;
#3132 = AXIS2_PLACEMENT_3D ( 'NONE', #11251, #18766, #18523 ) ;
#3133 = CARTESIAN_POINT ( 'NONE',  ( -13.59981317924081701, 37.05039483956773694, -139.6306434366684357 ) ) ;
#3134 = EDGE_CURVE ( 'NONE', #21766, #5773, #23101, .T. ) ;
#3135 = CYLINDRICAL_SURFACE ( 'NONE', #3654, 7.500000000000005329 ) ;
#3136 = LINE ( 'NONE', #16093, #9380 ) ;
#3137 = CARTESIAN_POINT ( 'NONE',  ( 19.13369214879999802, 50.49999999980000354, -136.0552959530000123 ) ) ;
#3138 = VERTEX_POINT ( 'NONE', #4897 ) ;
#3139 = CARTESIAN_POINT ( 'NONE',  ( -10.66194399654457925, 33.15920395776767293, -144.2988335296967932 ) ) ;
#3140 = CARTESIAN_POINT ( 'NONE',  ( -0.2409605966970265190, 23.82477348803106310, -150.0552959529999839 ) ) ;
#3141 = CARTESIAN_POINT ( 'NONE',  ( -9.801780389418540906, 37.03339632396453851, -147.4803110669293176 ) ) ;
#3142 = CARTESIAN_POINT ( 'NONE',  ( -4.499999999959999109, 37.00000000000000000, -153.0552959529999839 ) ) ;
#3143 = ORIENTED_EDGE ( 'NONE', *, *, #15508, .F. ) ;
#3144 = CARTESIAN_POINT ( 'NONE',  ( 20.58976242830000203, -31.80400447969999789, -143.5552959529999839 ) ) ;
#3145 = EDGE_CURVE ( 'NONE', #18669, #3418, #20976, .T. ) ;
#3146 = ORIENTED_EDGE ( 'NONE', *, *, #21481, .T. ) ;
#3147 = CARTESIAN_POINT ( 'NONE',  ( -6.554568091467054991, 33.71641555244740829, -145.9835056079819822 ) ) ;
#3148 = PLANE ( 'NONE',  #23254 ) ;
#3149 = CARTESIAN_POINT ( 'NONE',  ( -21.19005019800000156, 41.30866696430000218, -143.6114845980000041 ) ) ;
#3150 = ADVANCED_FACE ( 'NONE', ( #4540 ), #4665, .F. ) ;
#3151 = VECTOR ( 'NONE', #15317, 1000.000000000000000 ) ;
#3152 = ORIENTED_EDGE ( 'NONE', *, *, #18916, .T. ) ;
#3153 = DIRECTION ( 'NONE',  ( 0.000000000000000000, 1.000000000000000000, 0.000000000000000000 ) ) ;
#3154 = CARTESIAN_POINT ( 'NONE',  ( 23.08797222880000177, -15.45109671570000032, -143.0552959529999839 ) ) ;
#3155 = VERTEX_POINT ( 'NONE', #15483 ) ;
#3156 = CARTESIAN_POINT ( 'NONE',  ( -21.70878449369999785, 39.52018264390000013, -147.4849246469999855 ) ) ;
#3157 = EDGE_CURVE ( 'NONE', #18609, #20700, #8334, .T. ) ;
#3158 = CARTESIAN_POINT ( 'NONE',  ( 18.66051412330858383, 24.90191174486891867, -150.0552959529999839 ) ) ;
#3159 = EDGE_CURVE ( 'NONE', #1590, #1140, #22873, .T. ) ;
#3160 = PLANE ( 'NONE',  #3671 ) ;
#3161 = CARTESIAN_POINT ( 'NONE',  ( -12.28014746100000032, 36.97113097969999984, -148.4919582129999753 ) ) ;
#3162 = ADVANCED_FACE ( 'NONE', ( #22986 ), #17740, .F. ) ;
#3163 = DIRECTION ( 'NONE',  ( 1.000000000000000000, 0.000000000000000000, -2.257157423930000049E-12 ) ) ;
#3164 = CARTESIAN_POINT ( 'NONE',  ( -16.37184312240000139, 32.37338091950000063, -144.3414871020000021 ) ) ;
#3165 = CARTESIAN_POINT ( 'NONE',  ( -4.946601369560000627, -23.77962690289999870, -144.0552959529999839 ) ) ;
#3166 = DIRECTION ( 'NONE',  ( 0.1985297072190585210, 0.9800948705872890576, -8.351208274002460500E-13 ) ) ;
#3167 = VERTEX_POINT ( 'NONE', #11782 ) ;
#3168 = LINE ( 'NONE', #13980, #18931 ) ;
#3169 = EDGE_LOOP ( 'NONE', ( #1224, #11127, #9310 ) ) ;
#3170 = EDGE_LOOP ( 'NONE', ( #22135, #900, #9249, #17936, #11292 ) ) ;
#3171 = PLANE ( 'NONE',  #18577 ) ;
#3172 = LINE ( 'NONE', #13873, #5388 ) ;
#3173 = VERTEX_POINT ( 'NONE', #2770 ) ;
#3174 = EDGE_LOOP ( 'NONE', ( #2231, #8769, #20425, #47 ) ) ;
#3175 = DIRECTION ( 'NONE',  ( 0.000000000000000000, 0.000000000000000000, 1.000000000000000000 ) ) ;
#3176 = CARTESIAN_POINT ( 'NONE',  ( -19.09494877090000031, 33.54410563159999725, -142.1858765940000069 ) ) ;
#3177 = DIRECTION ( 'NONE',  ( 4.430318231639999944E-12, -6.100259101500000139E-13, 1.000000000000000000 ) ) ;
#3178 = B_SPLINE_CURVE_WITH_KNOTS ( 'NONE', 3,
 ( #4292, #2626, #15814, #10332 ),
 .UNSPECIFIED., .F., .F.,
 ( 4, 4 ),
 ( 0.000000000000000000, 0.8059436278830001132 ),
 .UNSPECIFIED. ) ;
#3179 = AXIS2_PLACEMENT_3D ( 'NONE', #7456, #14611, #18519 ) ;
#3180 = CARTESIAN_POINT ( 'NONE',  ( 24.85988213910000155, -26.16224997189999968, -145.5552959529999839 ) ) ;
#3181 = CARTESIAN_POINT ( 'NONE',  ( -7.033127412180307125, 32.99152251563850768, -141.7906166089485396 ) ) ;
#3182 = ORIENTED_EDGE ( 'NONE', *, *, #7620, .T. ) ;
#3183 = DIRECTION ( 'NONE',  ( 0.000000000000000000, 0.000000000000000000, 1.000000000000000000 ) ) ;
#3184 = EDGE_CURVE ( 'NONE', #7540, #21170, #14994, .T. ) ;
#3185 = DIRECTION ( 'NONE',  ( 0.000000000000000000, 0.000000000000000000, 1.000000000000000000 ) ) ;
#3186 = DIRECTION ( 'NONE',  ( 1.000000000000000000, 0.000000000000000000, 2.507771768019999718E-12 ) ) ;
#3187 = ORIENTED_EDGE ( 'NONE', *, *, #20709, .F. ) ;
#3188 = CARTESIAN_POINT ( 'NONE',  ( -22.10824191589999899, -4.000000000000000000, -141.0657682190000060 ) ) ;
#3189 = ORIENTED_EDGE ( 'NONE', *, *, #12349, .F. ) ;
#3190 = CARTESIAN_POINT ( 'NONE',  ( -21.03694116389999635, 36.94210036639999828, -147.9486865819999935 ) ) ;
#3191 = CYLINDRICAL_SURFACE ( 'NONE', #10849, 1.500000000000001332 ) ;
#3192 = EDGE_LOOP ( 'NONE', ( #1448, #11981, #6114, #6171 ) ) ;
#3193 = CARTESIAN_POINT ( 'NONE',  ( -22.56584646749552903, 37.05444931710232481, -139.6092474952423288 ) ) ;
#3194 = CARTESIAN_POINT ( 'NONE',  ( -10.65913935279999869, 37.04331329920000115, -139.7140392919999954 ) ) ;
#3195 = ORIENTED_EDGE ( 'NONE', *, *, #7805, .F. ) ;
#3196 = CARTESIAN_POINT ( 'NONE',  ( -15.37212823710000009, 38.89807584180000077, -148.3010324070000081 ) ) ;
#3197 = CARTESIAN_POINT ( 'NONE',  ( -24.76223978037774032, 32.81123456503314628, -146.4711376325379604 ) ) ;
#3198 = EDGE_LOOP ( 'NONE', ( #4763, #9828, #8564, #21855 ) ) ;
#3199 = ORIENTED_EDGE ( 'NONE', *, *, #20009, .T. ) ;
#3200 = CARTESIAN_POINT ( 'NONE',  ( -12.30631862549999944, 40.23402543379999230, -145.9987124289999940 ) ) ;
#3201 = EDGE_CURVE ( 'NONE', #20903, #16332, #17273, .T. ) ;
#3202 = CARTESIAN_POINT ( 'NONE',  ( -9.434278515689999978, -18.41834002140000237, -146.5552959529999839 ) ) ;
#3203 = VERTEX_POINT ( 'NONE', #6440 ) ;
#3204 = FACE_OUTER_BOUND ( 'NONE', #19712, .T. ) ;
#3205 = EDGE_CURVE ( 'NONE', #16693, #21987, #19293, .T. ) ;
#3206 = EDGE_CURVE ( 'NONE', #11665, #21515, #1103, .T. ) ;
#3207 = LINE ( 'NONE', #19264, #2999 ) ;
#3208 = ORIENTED_EDGE ( 'NONE', *, *, #20168, .T. ) ;
#3209 = DIRECTION ( 'NONE',  ( 2.257144641399999941E-12, 0.000000000000000000, 1.000000000000000000 ) ) ;
#3210 = EDGE_CURVE ( 'NONE', #13163, #3680, #12023, .T. ) ;
#3211 = AXIS2_PLACEMENT_3D ( 'NONE', #15260, #22396, #22517 ) ;
#3212 = ORIENTED_EDGE ( 'NONE', *, *, #14784, .F. ) ;
#3213 = FACE_OUTER_BOUND ( 'NONE', #8069, .T. ) ;
#3214 = CARTESIAN_POINT ( 'NONE',  ( -9.999999999959999997, 25.50000000000000000, -136.0552959530000123 ) ) ;
#3215 = CARTESIAN_POINT ( 'NONE',  ( -14.19189821223558567, 41.34771858761131824, -144.5672307995002939 ) ) ;
#3216 = DIRECTION ( 'NONE',  ( -0.9954742291034677226, 0.09503188512734457583, 4.503363594322118746E-12 ) ) ;
#3217 = EDGE_LOOP ( 'NONE', ( #985, #5840, #3336, #1391 ) ) ;
#3218 = PRESENTATION_STYLE_ASSIGNMENT (( #12246 ) ) ;
#3219 = DIRECTION ( 'NONE',  ( 2.326943610902514898E-15, 0.000000000000000000, 1.000000000000000000 ) ) ;
#3220 = DIRECTION ( 'NONE',  ( 1.000000000000000000, -5.094701932209999624E-24, 0.000000000000000000 ) ) ;
#3221 = CARTESIAN_POINT ( 'NONE',  ( 32.50000000000000000, 32.96379895120000469, -137.0552959530000123 ) ) ;
#3222 = CARTESIAN_POINT ( 'NONE',  ( 24.68320006080000084, -24.50000000000000000, -148.5552959529999839 ) ) ;
#3223 = CARTESIAN_POINT ( 'NONE',  ( -34.97299999999999898, 16.19395640470000330, -142.8567321060000097 ) ) ;
#3224 = EDGE_LOOP ( 'NONE', ( #19194, #10658, #15312, #9213 ) ) ;
#3225 = DIRECTION ( 'NONE',  ( 1.000000000000000000, 0.000000000000000000, -2.257171095940000041E-12 ) ) ;
#3226 = CARTESIAN_POINT ( 'NONE',  ( -8.296392858609999976, -9.821782169089999570, -148.5552959529999839 ) ) ;
#3227 = FACE_OUTER_BOUND ( 'NONE', #13579, .T. ) ;
#3228 = CARTESIAN_POINT ( 'NONE',  ( -1.499999999969999998, 44.50000000000000000, -136.5552959530000123 ) ) ;
#3229 = CARTESIAN_POINT ( 'NONE',  ( 1.591914056710000080, -18.48847405160000079, -143.5552959529999839 ) ) ;
#3230 = ORIENTED_EDGE ( 'NONE', *, *, #7654, .F. ) ;
#3231 = ADVANCED_FACE ( 'NONE', ( #10237 ), #13934, .F. ) ;
#3232 = DIRECTION ( 'NONE',  ( 0.000000000000000000, 0.000000000000000000, 1.000000000000000000 ) ) ;
#3233 = CARTESIAN_POINT ( 'NONE',  ( 32.50000000000000000, 20.96379895120000114, -136.0552959530000123 ) ) ;
#3234 = EDGE_CURVE ( 'NONE', #6536, #11683, #23450, .T. ) ;
#3235 = VERTEX_POINT ( 'NONE', #10937 ) ;
#3236 = CARTESIAN_POINT ( 'NONE',  ( -29.58443045183165410, 36.11526935725738241, -140.1709594658998981 ) ) ;
#3237 = CARTESIAN_POINT ( 'NONE',  ( -13.86630785130000021, 51.00000000000000000, -136.0552959530000123 ) ) ;
#3238 = ORIENTED_EDGE ( 'NONE', *, *, #7901, .T. ) ;
#3239 = CARTESIAN_POINT ( 'NONE',  ( -24.65454682284185139, 38.48142452593771168, -147.3520111327411257 ) ) ;
#3240 = DIRECTION ( 'NONE',  ( 1.000000000000000000, 0.000000000000000000, -2.257453483404485639E-12 ) ) ;
#3241 = CARTESIAN_POINT ( 'NONE',  ( -32.50000000000000000, 48.00000000000000000, -146.5552959529999839 ) ) ;
#3242 = CARTESIAN_POINT ( 'NONE',  ( 7.665856076347231429, 38.24667833328184230, -141.8883195129079979 ) ) ;
#3243 = VECTOR ( 'NONE', #11888, 1000.000000000000000 ) ;
#3244 = EDGE_LOOP ( 'NONE', ( #10415, #23135, #10407, #7914 ) ) ;
#3245 = CARTESIAN_POINT ( 'NONE',  ( -4.584402860569999127, 37.05223431090000474, -140.2914745300000163 ) ) ;
#3246 = DIRECTION ( 'NONE',  ( -0.2208456705930775810, -0.9753087663813413410, 1.089717887850382194E-12 ) ) ;
#3247 = CARTESIAN_POINT ( 'NONE',  ( 6.500000000040000003, 20.50000000000000000, -136.0552959530000123 ) ) ;
#3248 = CARTESIAN_POINT ( 'NONE',  ( 6.148946002053968130, -30.79517854816079137, -136.0552959530138821 ) ) ;
#3249 = ORIENTED_EDGE ( 'NONE', *, *, #15929, .T. ) ;
#3250 =( NAMED_UNIT ( * ) PLANE_ANGLE_UNIT ( ) SI_UNIT ( $, .RADIAN. ) );
#3251 = EDGE_CURVE ( 'NONE', #20598, #12734, #9271, .T. ) ;
#3252 = EDGE_LOOP ( 'NONE', ( #15305, #13897, #15340, #2662 ) ) ;
#3253 = CARTESIAN_POINT ( 'NONE',  ( -8.360775440490805011, 36.18761969327825767, -140.5275716988375336 ) ) ;
#3254 = CARTESIAN_POINT ( 'NONE',  ( -7.010349701930000066, 37.05829245179999987, -148.1453878979999956 ) ) ;
#3255 = LINE ( 'NONE', #15637, #7386 ) ;
#3256 = ORIENTED_EDGE ( 'NONE', *, *, #12141, .F. ) ;
#3257 = DIRECTION ( 'NONE',  ( 1.000000000000000000, 0.000000000000000000, -4.431640239962082113E-12 ) ) ;
#3258 = CARTESIAN_POINT ( 'NONE',  ( -21.35824191589999899, -32.00000000000000000, -150.0657682190000060 ) ) ;
#3259 = VECTOR ( 'NONE', #12128, 1000.000000000000000 ) ;
#3260 = EDGE_CURVE ( 'NONE', #15679, #7495, #16718, .T. ) ;
#3261 = ORIENTED_EDGE ( 'NONE', *, *, #3666, .F. ) ;
#3262 = CARTESIAN_POINT ( 'NONE',  ( -16.91592704299999994, 37.75347730500000409, -140.5160138910000001 ) ) ;
#3263 = DIRECTION ( 'NONE',  ( 0.000000000000000000, 0.000000000000000000, -1.000000000000000000 ) ) ;
#3264 = DIRECTION ( 'NONE',  ( 2.257144641399999941E-12, 0.000000000000000000, 1.000000000000000000 ) ) ;
#3265 = CARTESIAN_POINT ( 'NONE',  ( 7.014880255720557400, -46.74993274156790335, -136.0552959530158716 ) ) ;
#3266 = FACE_OUTER_BOUND ( 'NONE', #9472, .T. ) ;
#3267 = ADVANCED_FACE ( 'NONE', ( #12732 ), #9156, .T. ) ;
#3268 = CARTESIAN_POINT ( 'NONE',  ( -16.48779918059999616, 32.42295671489999620, -143.3618442240000093 ) ) ;
#3269 = APPLICATION_PROTOCOL_DEFINITION ( 'draft international standard', 'automotive_design', 1998, #16784 ) ;
#3270 = LINE ( 'NONE', #21130, #8236 ) ;
#3271 = FACE_OUTER_BOUND ( 'NONE', #10038, .T. ) ;
#3272 = ORIENTED_EDGE ( 'NONE', *, *, #20794, .T. ) ;
#3273 = VECTOR ( 'NONE', #14136, 1000.000000000000000 ) ;
#3274 = PLANE ( 'NONE',  #9800 ) ;
#3275 = AXIS2_PLACEMENT_3D ( 'NONE', #3625, #9194, #173 ) ;
#3276 = EDGE_LOOP ( 'NONE', ( #22085, #12399, #12926, #12667 ) ) ;
#3277 = EDGE_CURVE ( 'NONE', #154, #11758, #4731, .T. ) ;
#3278 = EDGE_CURVE ( 'NONE', #4889, #10478, #6914, .T. ) ;
#3279 = VERTEX_POINT ( 'NONE', #21915 ) ;
#3280 = CARTESIAN_POINT ( 'NONE',  ( 8.900000000049999471, 37.00000000000000000, -148.7552959530000010 ) ) ;
#3281 = DIRECTION ( 'NONE',  ( 1.000000000000000000, 0.000000000000000000, -2.256131789327550371E-12 ) ) ;
#3282 = ORIENTED_EDGE ( 'NONE', *, *, #9812, .F. ) ;
#3283 = EDGE_CURVE ( 'NONE', #19376, #1427, #18340, .T. ) ;
#3284 = VERTEX_POINT ( 'NONE', #20004 ) ;
#3285 = CARTESIAN_POINT ( 'NONE',  ( -7.500000000000000000, 19.50000000000000000, -150.0552959529999839 ) ) ;
#3286 = EDGE_CURVE ( 'NONE', #30, #22422, #2831, .T. ) ;
#3287 = LINE ( 'NONE', #4960, #771 ) ;
#3288 = CARTESIAN_POINT ( 'NONE',  ( -11.57053722856168321, 40.11345306623577756, -146.0212872837172711 ) ) ;
#3289 = FACE_OUTER_BOUND ( 'NONE', #2203, .T. ) ;
#3290 = ORIENTED_EDGE ( 'NONE', *, *, #15799, .F. ) ;
#3291 = FACE_OUTER_BOUND ( 'NONE', #21899, .T. ) ;
#3292 = ADVANCED_BREP_SHAPE_REPRESENTATION ( '', ( #11774, #5025 ), #8794 ) ;
#3293 = VERTEX_POINT ( 'NONE', #26 ) ;
#3294 = CARTESIAN_POINT ( 'NONE',  ( 9.634600858332637685, 36.01766042586972816, -141.7561022817950800 ) ) ;
#3295 = VECTOR ( 'NONE', #5631, 1000.000000000000000 ) ;
#3296 = CARTESIAN_POINT ( 'NONE',  ( -8.462973826026381374, 36.94736262684724437, -140.5165674475847197 ) ) ;
#3297 = CARTESIAN_POINT ( 'NONE',  ( 5.792747474889999637, -16.92794981449999980, -144.5552959529999839 ) ) ;
#3298 = ORIENTED_EDGE ( 'NONE', *, *, #8919, .T. ) ;
#3299 = DIRECTION ( 'NONE',  ( 2.257115129720000004E-12, 0.000000000000000000, 1.000000000000000000 ) ) ;
#3300 = ORIENTED_EDGE ( 'NONE', *, *, #14055, .T. ) ;
#3301 = CARTESIAN_POINT ( 'NONE',  ( -6.683153925719999222, 51.50000000000000000, -150.0552959529999839 ) ) ;
#3302 = FACE_OUTER_BOUND ( 'NONE', #3780, .T. ) ;
#3304 = ORIENTED_EDGE ( 'NONE', *, *, #6206, .T. ) ;
#3303 = VECTOR ( 'NONE', #15149, 1000.000000000000000 ) ;
#3305 = LINE ( 'NONE', #1658, #10696 ) ;
#3306 = ORIENTED_EDGE ( 'NONE', *, *, #1983, .F. ) ;
#3307 = CARTESIAN_POINT ( 'NONE',  ( -22.31464002779999944, 34.51618902799999944, -147.4864127260000259 ) ) ;
#3308 = EDGE_CURVE ( 'NONE', #8795, #9023, #20124, .T. ) ;
#3309 = VECTOR ( 'NONE', #16755, 1000.000000000000000 ) ;
#3310 = CARTESIAN_POINT ( 'NONE',  ( -4.020716686263415163, 46.44926652720589999, -136.0552959529909174 ) ) ;
#3311 = ORIENTED_EDGE ( 'NONE', *, *, #20813, .F. ) ;
#3312 = DIRECTION ( 'NONE',  ( 1.000000000000000000, 0.000000000000000000, 0.000000000000000000 ) ) ;
#3313 = ORIENTED_EDGE ( 'NONE', *, *, #3080, .T. ) ;
#3314 = LINE ( 'NONE', #14505, #11352 ) ;
#3315 = DIRECTION ( 'NONE',  ( 0.000000000000000000, -4.148443855749999753E-27, -1.000000000000000000 ) ) ;
#3316 = EDGE_LOOP ( 'NONE', ( #8032, #3427, #1295, #5835 ) ) ;
#3317 = CARTESIAN_POINT ( 'NONE',  ( 4.750000000000000000, -47.00000000000000000, -151.0552959529999839 ) ) ;
#3318 = CARTESIAN_POINT ( 'NONE',  ( -4.021770264099999714, -29.17051924670000318, -143.5552959529999839 ) ) ;
#3319 = ORIENTED_EDGE ( 'NONE', *, *, #17732, .F. ) ;
#3320 = CARTESIAN_POINT ( 'NONE',  ( -2.979194667911468919, 46.44907581354189574, -150.0552959529999839 ) ) ;
#3321 = AXIS2_PLACEMENT_3D ( 'NONE', #2489, #20926, #17221 ) ;
#3322 = AXIS2_PLACEMENT_3D ( 'NONE', #17018, #2521, #2414 ) ;
#3323 = ORIENTED_EDGE ( 'NONE', *, *, #20640, .T. ) ;
#3324 = CARTESIAN_POINT ( 'NONE',  ( 32.50000000000000000, -2.273736754430000208E-12, -136.0552959530000123 ) ) ;
#3325 = CARTESIAN_POINT ( 'NONE',  ( -5.316799939240000938, 3.500000000000000000, -149.3052959529999839 ) ) ;
#3326 = CARTESIAN_POINT ( 'NONE',  ( -14.87492916135365384, 38.44269649874472350, -147.4253129834213780 ) ) ;
#3327 = DIRECTION ( 'NONE',  ( -1.211690350418039921E-27, -2.765629237168040089E-27, 1.000000000000000000 ) ) ;
#3328 = ORIENTED_EDGE ( 'NONE', *, *, #16339, .T. ) ;
#3329 = LINE ( 'NONE', #23439, #6744 ) ;
#3330 = LINE ( 'NONE', #4881, #13501 ) ;
#3331 = FACE_BOUND ( 'NONE', #9585, .T. ) ;
#3332 = CARTESIAN_POINT ( 'NONE',  ( -18.35824191589999899, -1.500000000000000000, -141.0657682190000060 ) ) ;
#3333 = CARTESIAN_POINT ( 'NONE',  ( -24.50448663620845480, 36.99790949616351554, -147.3823814621291888 ) ) ;
#3334 = EDGE_CURVE ( 'NONE', #4867, #6268, #5596, .T. ) ;
#3335 = DIRECTION ( 'NONE',  ( 0.000000000000000000, 1.000000000000000000, 0.000000000000000000 ) ) ;
#3336 = ORIENTED_EDGE ( 'NONE', *, *, #4732, .T. ) ;
#3337 = CARTESIAN_POINT ( 'NONE',  ( 8.750000000030000891, -36.98606797749999942, -136.0552959530000123 ) ) ;
#3338 = VECTOR ( 'NONE', #7879, 1000.000000000000000 ) ;
#3339 = DIRECTION ( 'NONE',  ( -0.7071067811865473507, 0.7071067811865476838, 1.591319668629389897E-12 ) ) ;
#3340 = DIRECTION ( 'NONE',  ( -1.526468026909999897E-13, -8.159623473500000156E-13, -1.000000000000000000 ) ) ;
#3341 = VECTOR ( 'NONE', #10644, 1000.000000000000000 ) ;
#3342 = CARTESIAN_POINT ( 'NONE',  ( -6.166004029562527577, 36.95750611116528717, -148.6250205690956534 ) ) ;
#3343 = CARTESIAN_POINT ( 'NONE',  ( -30.49999999990282262, 39.50000000000000000, -144.0552959529548502 ) ) ;
#3344 = DIRECTION ( 'NONE',  ( -1.525446435830000185E-13, -8.171241461240000022E-13, -1.000000000000000000 ) ) ;
#3345 = EDGE_LOOP ( 'NONE', ( #21709, #3988, #14253, #8703 ) ) ;
#3346 = DIRECTION ( 'NONE',  ( 0.1000233216789610108, 0.9949850929136109245, -3.588240815588595806E-13 ) ) ;
#3347 = LINE ( 'NONE', #22878, #10181 ) ;
#3348 = ORIENTED_EDGE ( 'NONE', *, *, #5333, .T. ) ;
#3349 = DIRECTION ( 'NONE',  ( 1.000000000000000000, 0.000000000000000000, -4.431640239962082113E-12 ) ) ;
#3350 = EDGE_LOOP ( 'NONE', ( #19538, #6492, #10581 ) ) ;
#3351 = LINE ( 'NONE', #6926, #20502 ) ;
#3352 = CIRCLE ( 'NONE', #21233, 2.500000000000000444 ) ;
#3353 = FACE_OUTER_BOUND ( 'NONE', #2471, .T. ) ;
#3354 = AXIS2_PLACEMENT_3D ( 'NONE', #14225, #21490, #20149 ) ;
#3355 = CARTESIAN_POINT ( 'NONE',  ( -7.499999999959999997, 42.50000000000000000, -136.0552959530000123 ) ) ;
#3356 = CARTESIAN_POINT ( 'NONE',  ( 7.306041003437069747, 37.90825656058944304, -141.7260982854917017 ) ) ;
#3357 = ORIENTED_EDGE ( 'NONE', *, *, #12944, .T. ) ;
#3358 = DIRECTION ( 'NONE',  ( 0.000000000000000000, 1.000000000000000000, 0.000000000000000000 ) ) ;
#3359 = CARTESIAN_POINT ( 'NONE',  ( -18.95027878879999861, 36.16636532760000478, -148.4341920939999966 ) ) ;
#3360 = DIRECTION ( 'NONE',  ( 2.257144641399999941E-12, -8.049635380228619169E-35, 1.000000000000000000 ) ) ;
#3361 = CARTESIAN_POINT ( 'NONE',  ( 31.50000000000000000, 39.80430157320000006, -143.0552959529999839 ) ) ;
#3362 = EDGE_CURVE ( 'NONE', #1359, #20086, #21685, .T. ) ;
#3363 = ORIENTED_EDGE ( 'NONE', *, *, #13746, .T. ) ;
#3364 = EDGE_CURVE ( 'NONE', #17304, #11140, #3467, .T. ) ;
#3365 = FACE_OUTER_BOUND ( 'NONE', #8140, .T. ) ;
#3366 =( NAMED_UNIT ( * ) SI_UNIT ( $, .STERADIAN. ) SOLID_ANGLE_UNIT ( ) );
#3367 = ORIENTED_EDGE ( 'NONE', *, *, #19262, .T. ) ;
#3368 = CARTESIAN_POINT ( 'NONE',  ( -9.347107914279998653, -17.32706600430000066, -143.5552959529999839 ) ) ;
#3369 = DIRECTION ( 'NONE',  ( 1.526468026909999897E-13, 8.159623473500000156E-13, 1.000000000000000000 ) ) ;
#3370 = DIRECTION ( 'NONE',  ( -0.9954742291034676116, 0.09503188512734456195, 0.000000000000000000 ) ) ;
#3371 = VECTOR ( 'NONE', #1048, 1000.000000000000000 ) ;
#3372 = ORIENTED_EDGE ( 'NONE', *, *, #17087, .F. ) ;
#3373 = DIRECTION ( 'NONE',  ( 4.430318231639999944E-12, -6.100259101500000139E-13, 1.000000000000000000 ) ) ;
#3374 = FACE_OUTER_BOUND ( 'NONE', #13985, .T. ) ;
#3375 = CIRCLE ( 'NONE', #338, 0.7500000000000006661 ) ;
#3376 = ORIENTED_EDGE ( 'NONE', *, *, #9089, .T. ) ;
#3377 = CARTESIAN_POINT ( 'NONE',  ( -16.79401156879999846, -18.00000000000000000, -148.8157682190000060 ) ) ;
#3378 = VECTOR ( 'NONE', #1850, 1000.000000000000000 ) ;
#3379 = VECTOR ( 'NONE', #4751, 1000.000000000000000 ) ;
#3380 = CARTESIAN_POINT ( 'NONE',  ( 17.49993271304850140, 22.89748944252527352, -150.0552959529999839 ) ) ;
#3381 = CARTESIAN_POINT ( 'NONE',  ( -16.50000000000000000, -43.00000000000000000, -150.0552959529999839 ) ) ;
#3382 = DIRECTION ( 'NONE',  ( 0.000000000000000000, 1.000000000000000000, 0.000000000000000000 ) ) ;
#3383 = PLANE ( 'NONE',  #23080 ) ;
#3384 = FACE_OUTER_BOUND ( 'NONE', #20907, .T. ) ;
#3385 = CARTESIAN_POINT ( 'NONE',  ( -1.552054646623368228, 43.97650423128144581, -136.0552959530043893 ) ) ;
#3386 = AXIS2_PLACEMENT_3D ( 'NONE', #7523, #1966, #14677 ) ;
#3387 = VECTOR ( 'NONE', #12038, 1000.000000000000000 ) ;
#3388 = ORIENTED_EDGE ( 'NONE', *, *, #3978, .T. ) ;
#3389 = EDGE_CURVE ( 'NONE', #19876, #11512, #16315, .T. ) ;
#3390 = ORIENTED_EDGE ( 'NONE', *, *, #1097, .F. ) ;
#3391 = PRESENTATION_STYLE_ASSIGNMENT (( #7083 ) ) ;
#3392 = VECTOR ( 'NONE', #6509, 1000.000000000000000 ) ;
#3393 = EDGE_LOOP ( 'NONE', ( #22080, #3272, #20503, #5083 ) ) ;
#3394 = DIRECTION ( 'NONE',  ( 0.000000000000000000, 1.000000000000000000, 0.000000000000000000 ) ) ;
#3395 = CARTESIAN_POINT ( 'NONE',  ( -27.99900835291655810, 33.07904996078797666, -141.6633825115897025 ) ) ;
#3396 = VERTEX_POINT ( 'NONE', #7270 ) ;
#3397 = PLANE ( 'NONE',  #22069 ) ;
#3398 = ORIENTED_EDGE ( 'NONE', *, *, #15067, .T. ) ;
#3399 = CARTESIAN_POINT ( 'NONE',  ( 32.00000000000000000, -21.03620104879999886, -136.0552959530000123 ) ) ;
#3400 = EDGE_CURVE ( 'NONE', #11681, #10143, #23337, .T. ) ;
#3401 = CARTESIAN_POINT ( 'NONE',  ( -18.92206117636284546, 33.99949261441817328, -145.9371503374987356 ) ) ;
#3402 = PLANE ( 'NONE',  #2407 ) ;
#3403 = CARTESIAN_POINT ( 'NONE',  ( 31.50000000000000000, -2.273736754430000208E-12, -136.0552959530000123 ) ) ;
#3404 = ORIENTED_EDGE ( 'NONE', *, *, #10243, .T. ) ;
#3405 = FACE_BOUND ( 'NONE', #14693, .T. ) ;
#3406 = CIRCLE ( 'NONE', #2289, 5.000000000000000000 ) ;
#3407 = APPLICATION_CONTEXT ( 'automotive_design' ) ;
#3408 = ORIENTED_EDGE ( 'NONE', *, *, #18526, .T. ) ;
#3409 = AXIS2_PLACEMENT_3D ( 'NONE', #10447, #10798, #19875 ) ;
#3410 = CARTESIAN_POINT ( 'NONE',  ( 10.68320006080000084, -20.50000000000000000, -148.5552959529999839 ) ) ;
#3411 = CIRCLE ( 'NONE', #22403, 0.5000000000000004441 ) ;
#3412 = ADVANCED_FACE ( 'NONE', ( #16199 ), #5243, .F. ) ;
#3413 = LINE ( 'NONE', #14359, #21256 ) ;
#3414 = AXIS2_PLACEMENT_3D ( 'NONE', #1800, #11162, #4039 ) ;
#3415 = VECTOR ( 'NONE', #7837, 1000.000000000000000 ) ;
#3416 = EDGE_CURVE ( 'NONE', #416, #1359, #17986, .T. ) ;
#3417 = CARTESIAN_POINT ( 'NONE',  ( 0.8371776177479999248, 14.00000000000000000, -144.0552959529999839 ) ) ;
#3418 = VERTEX_POINT ( 'NONE', #9729 ) ;
#3419 = EDGE_CURVE ( 'NONE', #16273, #6526, #18796, .T. ) ;
#3420 = ADVANCED_FACE ( 'NONE', ( #18560 ), #11406, .F. ) ;
#3421 = PLANE ( 'NONE',  #5734 ) ;
#3422 = ORIENTED_EDGE ( 'NONE', *, *, #17495, .F. ) ;
#3423 = CARTESIAN_POINT ( 'NONE',  ( -7.499999999969999109, 25.50000000000000000, -137.0552959530000123 ) ) ;
#3424 = CYLINDRICAL_SURFACE ( 'NONE', #11993, 0.9999999999999950040 ) ;
#3425 = ORIENTED_EDGE ( 'NONE', *, *, #23166, .T. ) ;
#3426 = CARTESIAN_POINT ( 'NONE',  ( 25.34364015992475316, -22.89900052719453427, -150.0552959529999839 ) ) ;
#3427 = ORIENTED_EDGE ( 'NONE', *, *, #8344, .F. ) ;
#3428 = CARTESIAN_POINT ( 'NONE',  ( -15.96254761875824180, 38.65457006438045795, -147.5807964054747856 ) ) ;
#3429 = CARTESIAN_POINT ( 'NONE',  ( -29.36832786400000117, 38.86294434210000048, -140.8528603229999874 ) ) ;
#3430 = ORIENTED_EDGE ( 'NONE', *, *, #2459, .T. ) ;
#3431 = VECTOR ( 'NONE', #23044, 1000.000000000000000 ) ;
#3432 = AXIS2_PLACEMENT_3D ( 'NONE', #3989, #13378, #7778 ) ;
#3433 = ORIENTED_EDGE ( 'NONE', *, *, #8802, .T. ) ;
#3434 = AXIS2_PLACEMENT_3D ( 'NONE', #3970, #16814, #5859 ) ;
#3435 = CARTESIAN_POINT ( 'NONE',  ( -26.92295469378113992, 39.53966211714406143, -140.4202993119762368 ) ) ;
#3436 = EDGE_CURVE ( 'NONE', #6123, #2118, #669, .T. ) ;
#3437 = CARTESIAN_POINT ( 'NONE',  ( -31.50000000000000000, 1.000000000000000000, -149.5552959529999839 ) ) ;
#3438 = ORIENTED_EDGE ( 'NONE', *, *, #1335, .F. ) ;
#3439 = CARTESIAN_POINT ( 'NONE',  ( -32.50000000000000000, 19.50000000000000000, -150.5552959529999839 ) ) ;
#3440 = EDGE_CURVE ( 'NONE', #7907, #16321, #14757, .T. ) ;
#3441 = CARTESIAN_POINT ( 'NONE',  ( -10.65913935279999869, 37.04331329920000115, -139.7140392919999954 ) ) ;
#3442 = DIRECTION ( 'NONE',  ( 2.839308199620000013E-14, 3.568879590630000244E-13, 1.000000000000000000 ) ) ;
#3443 = EDGE_LOOP ( 'NONE', ( #7897, #4712, #9612, #19932, #9943, #22634 ) ) ;
#3444 = LINE ( 'NONE', #16519, #19338 ) ;
#3445 = EDGE_CURVE ( 'NONE', #12978, #8318, #13053, .T. ) ;
#3446 = EDGE_CURVE ( 'NONE', #20874, #3831, #1909, .T. ) ;
#3447 = EDGE_LOOP ( 'NONE', ( #8988, #4145, #18435, #19444, #19650, #22907, #18617 ) ) ;
#3448 = VECTOR ( 'NONE', #5360, 1000.000000000000227 ) ;
#3449 = AXIS2_PLACEMENT_3D ( 'NONE', #17447, #1176, #12437 ) ;
#3450 = DIRECTION ( 'NONE',  ( 0.000000000000000000, 0.000000000000000000, 1.000000000000000000 ) ) ;
#3451 = EDGE_CURVE ( 'NONE', #1104, #565, #16656, .T. ) ;
#3452 = CARTESIAN_POINT ( 'NONE',  ( -11.38486064697293898, 36.95668670074196172, -140.3965526142782210 ) ) ;
#3453 = CARTESIAN_POINT ( 'NONE',  ( -14.68945449529999969, 41.62249060810000145, -143.5408288559999903 ) ) ;
#3454 = ORIENTED_EDGE ( 'NONE', *, *, #8434, .F. ) ;
#3455 = LINE ( 'NONE', #8662, #6371 ) ;
#3456 = DIRECTION ( 'NONE',  ( -0.9840552701943220404, 0.1778629393740580045, -3.541738516501160129E-14 ) ) ;
#3457 = DIRECTION ( 'NONE',  ( 1.526468026909999897E-13, 8.159623473500000156E-13, 1.000000000000000000 ) ) ;
#3458 = FACE_OUTER_BOUND ( 'NONE', #12852, .T. ) ;
#3459 = LINE ( 'NONE', #12608, #1988 ) ;
#3460 = DIRECTION ( 'NONE',  ( -1.000000000000000000, 0.000000000000000000, 0.000000000000000000 ) ) ;
#3461 = ORIENTED_EDGE ( 'NONE', *, *, #20108, .F. ) ;
#3462 = DIRECTION ( 'NONE',  ( -2.257144641399999941E-12, 0.000000000000000000, -1.000000000000000000 ) ) ;
#3463 = DIRECTION ( 'NONE',  ( 2.257144641399999941E-12, -4.009147065140000298E-51, 1.000000000000000000 ) ) ;
#3464 = DIRECTION ( 'NONE',  ( 0.000000000000000000, -1.000000000000000000, -2.257144641399999941E-12 ) ) ;
#3465 = CARTESIAN_POINT ( 'NONE',  ( -4.626684792761640352, 38.75063101611807070, -140.2397901787329317 ) ) ;
#3466 = VECTOR ( 'NONE', #22093, 1000.000000000000000 ) ;
#3467 = LINE ( 'NONE', #12371, #4315 ) ;
#3468 = COLOUR_RGB ( '', 0.72549020, 0.75294118, 0.79215686) ;
#3469 = ORIENTED_EDGE ( 'NONE', *, *, #6101, .T. ) ;
#3470 = LINE ( 'NONE', #10707, #9434 ) ;
#3471 = CARTESIAN_POINT ( 'NONE',  ( -15.86078924153198599, 37.04043998683724226, -147.5134597624269190 ) ) ;
#3472 = ORIENTED_EDGE ( 'NONE', *, *, #3866, .F. ) ;
#3473 = EDGE_CURVE ( 'NONE', #17890, #2494, #11598, .T. ) ;
#3474 = EDGE_CURVE ( 'NONE', #20840, #3553, #16707, .T. ) ;
#3475 = CARTESIAN_POINT ( 'NONE',  ( 32.00000000000000000, 32.96379895120000469, -136.0552959530000123 ) ) ;
#3476 = ORIENTED_EDGE ( 'NONE', *, *, #4659, .T. ) ;
#3477 = CARTESIAN_POINT ( 'NONE',  ( -24.22614176569036459, 39.00041403165653975, -146.8502260740512213 ) ) ;
#3478 = CARTESIAN_POINT ( 'NONE',  ( -29.57566076271681510, 39.40610565237071228, -139.8786281328294763 ) ) ;
#3479 = DIRECTION ( 'NONE',  ( -0.9954742291034677226, 0.09503188512734457583, 4.502513436702118395E-12 ) ) ;
#3480 = CARTESIAN_POINT ( 'NONE',  ( 7.942238981814500498, 38.39246003580940680, -141.9790531659411101 ) ) ;
#3481 = VERTEX_POINT ( 'NONE', #18909 ) ;
#3482 = DIRECTION ( 'NONE',  ( 0.000000000000000000, -0.4794255386042033384, -0.8775825618903726477 ) ) ;
#3483 = VECTOR ( 'NONE', #670, 1000.000000000000000 ) ;
#3484 = VECTOR ( 'NONE', #7542, 1000.000000000000000 ) ;
#3485 = CARTESIAN_POINT ( 'NONE',  ( -19.48146791446731640, 32.28180044528915005, -143.8017659915034301 ) ) ;
#3486 = AXIS2_PLACEMENT_3D ( 'NONE', #3337, #8671, #15955 ) ;
#3487 = CARTESIAN_POINT ( 'NONE',  ( -9.341122566677128702, 40.18160354483676144, -145.8224011896586489 ) ) ;
#3488 = CARTESIAN_POINT ( 'NONE',  ( 4.798892695445801770, -31.45134726954360005, -136.0552959530108694 ) ) ;
#3489 = ORIENTED_EDGE ( 'NONE', *, *, #531, .F. ) ;
#3490 = DIRECTION ( 'NONE',  ( -0.8319143897030502055, -0.5549039990890329843, 3.347322419244847777E-12 ) ) ;
#3491 =( NAMED_UNIT ( * ) PLANE_ANGLE_UNIT ( ) SI_UNIT ( $, .RADIAN. ) );
#3492 = EDGE_LOOP ( 'NONE', ( #4975, #17946, #1517, #5112 ) ) ;
#3493 = LINE ( 'NONE', #12396, #17938 ) ;
#3494 = CARTESIAN_POINT ( 'NONE',  ( -23.24588518179999852, 41.24341284999999857, -143.7187626420000015 ) ) ;
#3495 = CARTESIAN_POINT ( 'NONE',  ( -32.50000000000000000, 26.00000000000000000, -137.5552959530000123 ) ) ;
#3496 = ORIENTED_EDGE ( 'NONE', *, *, #1252, .F. ) ;
#3497 = LINE ( 'NONE', #5051, #14440 ) ;
#3498 = FACE_OUTER_BOUND ( 'NONE', #4609, .T. ) ;
#3499 = AXIS2_PLACEMENT_3D ( 'NONE', #11982, #9959, #20808 ) ;
#3500 = AXIS2_PLACEMENT_3D ( 'NONE', #22901, #20758, #2793 ) ;
#3501 = ORIENTED_EDGE ( 'NONE', *, *, #3717, .F. ) ;
#3502 = EDGE_CURVE ( 'NONE', #4852, #22736, #22796, .T. ) ;
#3503 = AXIS2_PLACEMENT_3D ( 'NONE', #12520, #21824, #18125 ) ;
#3504 = DIRECTION ( 'NONE',  ( 2.257144641397284947E-12, 2.714724913984255017E-24, 1.000000000000000000 ) ) ;
#3505 = EDGE_CURVE ( 'NONE', #7477, #14486, #11858, .T. ) ;
#3506 = CARTESIAN_POINT ( 'NONE',  ( 20.10199673422639322, 25.50000000000000355, -150.0552959529999839 ) ) ;
#3507 = DIRECTION ( 'NONE',  ( 1.000000000000000000, 0.000000000000000000, -2.253752739989067373E-12 ) ) ;
#3508 = ADVANCED_FACE ( 'NONE', ( #7955 ), #14991, .T. ) ;
#3509 = LINE ( 'NONE', #23142, #12900 ) ;
#3510 = CARTESIAN_POINT ( 'NONE',  ( -9.969904307360000217, -22.67446893780000039, -145.0552959529999839 ) ) ;
#3511 = CARTESIAN_POINT ( 'NONE',  ( -21.35824191589999899, -4.000000000000000000, -144.8157682190000060 ) ) ;
#3512 = CONTEXT_DEPENDENT_SHAPE_REPRESENTATION ( #217, #8387 ) ;
#3513 = DIRECTION ( 'NONE',  ( 0.000000000000000000, -1.000000000000000000, -2.273736754430000208E-12 ) ) ;
#3514 = CARTESIAN_POINT ( 'NONE',  ( 22.50000000000000000, 36.50000000000000000, -150.0552959529999839 ) ) ;
#3515 = CARTESIAN_POINT ( 'NONE',  ( 32.05742780220000299, -40.87448416729999678, -150.0552959529999839 ) ) ;
#3516 = ORIENTED_EDGE ( 'NONE', *, *, #20975, .T. ) ;
#3517 =( GEOMETRIC_REPRESENTATION_CONTEXT ( 3 ) GLOBAL_UNCERTAINTY_ASSIGNED_CONTEXT ( ( #20178 ) ) GLOBAL_UNIT_ASSIGNED_CONTEXT ( ( #15158, #6230, #13726 ) ) REPRESENTATION_CONTEXT ( 'NONE', 'WORKASPACE' ) );
#3518 = PRODUCT_DEFINITION_CONTEXT ( 'detailed design', #2963, 'design' ) ;
#3519 = VECTOR ( 'NONE', #15234, 1000.000000000000000 ) ;
#3520 = EDGE_CURVE ( 'NONE', #3906, #16283, #8539, .T. ) ;
#3521 = ORIENTED_EDGE ( 'NONE', *, *, #20709, .T. ) ;
#3522 = VERTEX_POINT ( 'NONE', #15348 ) ;
#3523 = CARTESIAN_POINT ( 'NONE',  ( -2.499999999940000439, 39.19395640469999620, -145.2538597999999865 ) ) ;
#3524 = DIRECTION ( 'NONE',  ( 0.6459422414661339928, -0.7633862853691482098, 0.000000000000000000 ) ) ;
#3525 = ORIENTED_EDGE ( 'NONE', *, *, #3128, .F. ) ;
#3526 = CARTESIAN_POINT ( 'NONE',  ( 23.99773978629999860, -29.25880395889999974, -147.5552959529999839 ) ) ;
#3527 = VERTEX_POINT ( 'NONE', #21181 ) ;
#3528 = DIRECTION ( 'NONE',  ( 1.000000000000000000, 0.000000000000000000, 0.000000000000000000 ) ) ;
#3529 = CARTESIAN_POINT ( 'NONE',  ( -19.34447215129067033, 33.98952392425853475, -145.9993797645266795 ) ) ;
#3530 = CARTESIAN_POINT ( 'NONE',  ( -11.48460281164964414, 40.77310199058896245, -146.4361868664954613 ) ) ;
#3531 = DIRECTION ( 'NONE',  ( -0.000000000000000000, 1.000000000000000000, 0.000000000000000000 ) ) ;
#3532 = ORIENTED_EDGE ( 'NONE', *, *, #5354, .F. ) ;
#3533 = CARTESIAN_POINT ( 'NONE',  ( 4.500000000009999113, -5.000000000000000000, -137.0552959530000123 ) ) ;
#3534 = VERTEX_POINT ( 'NONE', #12114 ) ;
#3535 = CARTESIAN_POINT ( 'NONE',  ( 8.549255091327660594, 35.49999999999985789, -142.0552959530001260 ) ) ;
#3536 =( GEOMETRIC_REPRESENTATION_CONTEXT ( 3 ) GLOBAL_UNCERTAINTY_ASSIGNED_CONTEXT ( ( #12778 ) ) GLOBAL_UNIT_ASSIGNED_CONTEXT ( ( #1720, #9723, #18552 ) ) REPRESENTATION_CONTEXT ( 'NONE', 'WORKASPACE' ) );
#3537 = EDGE_CURVE ( 'NONE', #19834, #8510, #4749, .T. ) ;
#3538 = VECTOR ( 'NONE', #15894, 1000.000000000000000 ) ;
#3539 = DIRECTION ( 'NONE',  ( 0.000000000000000000, -1.000000000000000000, 0.000000000000000000 ) ) ;
#3540 = LINE ( 'NONE', #14360, #4176 ) ;
#3541 = EDGE_LOOP ( 'NONE', ( #20081, #14631, #21867, #7152 ) ) ;
#3542 = PRODUCT_DEFINITION ( 'UNKNOWN', '', #9995, #14687 ) ;
#3543 = CARTESIAN_POINT ( 'NONE',  ( -20.60824191589999899, -4.000000000000000000, -150.0657682190000060 ) ) ;
#3544 = ORIENTED_EDGE ( 'NONE', *, *, #1462, .T. ) ;
#3545 = CARTESIAN_POINT ( 'NONE',  ( -19.79317654020000106, 38.64314174740000141, -140.5356700199999977 ) ) ;
#3546 = CARTESIAN_POINT ( 'NONE',  ( 0.000000000000000000, 0.000000000000000000, -140.0552959529999839 ) ) ;
#3547 = ORIENTED_EDGE ( 'NONE', *, *, #4558, .F. ) ;
#3548 = DIRECTION ( 'NONE',  ( -1.000000000000000000, 0.000000000000000000, 2.256683728769999802E-12 ) ) ;
#3549 = ORIENTED_EDGE ( 'NONE', *, *, #23043, .F. ) ;
#3550 = CARTESIAN_POINT ( 'NONE',  ( -31.50000000000000000, 16.00000000000000000, -144.0552959529999839 ) ) ;
#3551 = CARTESIAN_POINT ( 'NONE',  ( -4.726870213007021704, 46.10157554568331761, -136.0552959529892973 ) ) ;
#3552 = AXIS2_PLACEMENT_3D ( 'NONE', #214, #9584, #20085 ) ;
#3553 = VERTEX_POINT ( 'NONE', #20819 ) ;
#3554 = CARTESIAN_POINT ( 'NONE',  ( 0.000000000000000000, 0.000000000000000000, 0.000000000000000000 ) ) ;
#3555 = EDGE_CURVE ( 'NONE', #1038, #22422, #4868, .T. ) ;
#3556 = VERTEX_POINT ( 'NONE', #15813 ) ;
#3557 = CARTESIAN_POINT ( 'NONE',  ( -26.71298293347248887, 37.74538646634001537, -140.1185230284342538 ) ) ;
#3558 = CARTESIAN_POINT ( 'NONE',  ( 7.228490359739999427, -13.33508289800000135, -145.5552959529999839 ) ) ;
#3559 = ORIENTED_EDGE ( 'NONE', *, *, #20029, .T. ) ;
#3560 = DIRECTION ( 'NONE',  ( 0.000000000000000000, -1.000000000000000000, 0.000000000000000000 ) ) ;
#3561 = CARTESIAN_POINT ( 'NONE',  ( 16.16922456049999823, -22.27514461170000004, -147.5552959529999839 ) ) ;
#3562 = DIRECTION ( 'NONE',  ( 0.000000000000000000, 1.000000000000000000, 0.000000000000000000 ) ) ;
#3563 = ORIENTED_EDGE ( 'NONE', *, *, #11008, .F. ) ;
#3564 = DIRECTION ( 'NONE',  ( 1.000000000000000000, 0.000000000000000000, -2.254788948169999945E-12 ) ) ;
#3565 = EDGE_CURVE ( 'NONE', #16716, #18274, #8073, .T. ) ;
#3566 = ORIENTED_EDGE ( 'NONE', *, *, #15586, .F. ) ;
#3567 = DIRECTION ( 'NONE',  ( 3.882490197650000213E-51, -1.000000000000000000, -4.009147065150000317E-51 ) ) ;
#3568 = CARTESIAN_POINT ( 'NONE',  ( -10.65913935279999869, 37.04331329920000115, -139.7140392919999954 ) ) ;
#3569 = EDGE_CURVE ( 'NONE', #4645, #232, #1205, .T. ) ;
#3570 = CARTESIAN_POINT ( 'NONE',  ( -16.92431971701898874, 37.01165972487905265, -139.4624774945162358 ) ) ;
#3571 = DIRECTION ( 'NONE',  ( -2.507771768019999718E-12, -1.592654864209999947E-17, 1.000000000000000000 ) ) ;
#3572 = ORIENTED_EDGE ( 'NONE', *, *, #6653, .F. ) ;
#3573 = FILL_AREA_STYLE_COLOUR ( '', #22718 ) ;
#3574 = FACE_OUTER_BOUND ( 'NONE', #21255, .T. ) ;
#3575 = ADVANCED_FACE ( 'NONE', ( #10329 ), #5296, .F. ) ;
#3576 = CARTESIAN_POINT ( 'NONE',  ( 0.000000000000000000, 0.000000000000000000, -151.0552959529999839 ) ) ;
#3577 = DIRECTION ( 'NONE',  ( 1.000000000000000000, 0.000000000000000000, 0.000000000000000000 ) ) ;
#3578 = LINE ( 'NONE', #9021, #11073 ) ;
#3579 = CARTESIAN_POINT ( 'NONE',  ( -18.00000000000000000, -43.00000000000000000, -150.0552959529999839 ) ) ;
#3580 = ORIENTED_EDGE ( 'NONE', *, *, #9946, .F. ) ;
#3581 = CARTESIAN_POINT ( 'NONE',  ( 8.500000000050000892, 37.00000000000000000, -149.5552959529999839 ) ) ;
#3582 = EDGE_CURVE ( 'NONE', #18490, #7197, #9850, .T. ) ;
#3583 = DIRECTION ( 'NONE',  ( 5.094701932209999624E-24, 1.000000000000000000, 0.000000000000000000 ) ) ;
#3584 = CARTESIAN_POINT ( 'NONE',  ( -6.072796602490000417, -14.62912504250000012, -144.5552959529999839 ) ) ;
#3585 = EDGE_CURVE ( 'NONE', #5977, #21733, #22964, .T. ) ;
#3586 = CARTESIAN_POINT ( 'NONE',  ( -6.163071638762996685, 41.67289232386758613, -144.4686657573369644 ) ) ;
#3587 = CARTESIAN_POINT ( 'NONE',  ( -21.35824191589185972, -4.000000000000000000, -149.4708568729758724 ) ) ;
#3588 = EDGE_CURVE ( 'NONE', #7716, #16508, #21063, .T. ) ;
#3589 = ORIENTED_EDGE ( 'NONE', *, *, #15447, .T. ) ;
#3590 = AXIS2_PLACEMENT_3D ( 'NONE', #3035, #1363, #23249 ) ;
#3591 = DIRECTION ( 'NONE',  ( -3.994014902950000436E-29, 1.000000000000000000, -4.148443855749999753E-27 ) ) ;
#3592 = EDGE_CURVE ( 'NONE', #15090, #6658, #11014, .T. ) ;
#3593 = CARTESIAN_POINT ( 'NONE',  ( 8.750000000030000891, -44.75000000000000000, -137.0552959530000123 ) ) ;
#3594 = EDGE_LOOP ( 'NONE', ( #1608, #16064, #8873, #5714 ) ) ;
#3595 =( BOUNDED_SURFACE ( )  B_SPLINE_SURFACE ( 5, 5, ( 
 ( #21309, #3104, #21666, #17969, #23321, #14275 ),
 ( #5356, #12474, #5225, #23205, #10340, #1568 ),
 ( #5001, #19758, #19522, #1441, #14392, #8902 ),
 ( #14162, #21426, #7132, #18668, #14739, #12832 ),
 ( #18540, #3806, #19985, #7475, #11045, #18202 ),
 ( #22125, #11268, #2259, #2381, #10919, #1917 ),
 ( #584, #236, #18323, #4148, #13180, #13069 ),
 ( #18431, #20340, #3923, #349, #11157, #9602 ),
 ( #20230, #7591, #5580, #5811, #11386, #2145 ) ),
 .UNSPECIFIED., .F., .F., .F. ) 
 B_SPLINE_SURFACE_WITH_KNOTS ( ( 6, 3, 6 ),
 ( 6, 6 ),
 ( 0.000000000000000000, 5.731822293570000504, 9.005131590149998644 ),
 ( 1.570796326704904988, 3.141592653590000062 ),
 .UNSPECIFIED. ) 
 GEOMETRIC_REPRESENTATION_ITEM ( )  RATIONAL_B_SPLINE_SURFACE ( (
 ( 0.2500000000000000000, 0.2499999999885285096, 0.2999999999827930308, 0.3999999999770569858, 0.5999999999770569969, 1.000000000000000000),
 ( 0.2500000000000000000, 0.2499999999885285096, 0.2999999999827930308, 0.3999999999770569858, 0.5999999999770569969, 1.000000000000000000),
 ( 0.2500000000000000000, 0.2499999999885285096, 0.2999999999827930308, 0.3999999999770569858, 0.5999999999770569969, 1.000000000000000000),
 ( 0.2500000000000000000, 0.2499999999885285096, 0.2999999999827930308, 0.3999999999770569858, 0.5999999999770569969, 1.000000000000000000),
 ( 0.2500000000000000000, 0.2499999999885285096, 0.2999999999827930308, 0.3999999999770569858, 0.5999999999770569969, 1.000000000000000000),
 ( 0.2500000000000000000, 0.2499999999885285096, 0.2999999999827930308, 0.3999999999770569858, 0.5999999999770569969, 1.000000000000000000),
 ( 0.2500000000000000000, 0.2499999999885285096, 0.2999999999827930308, 0.3999999999770569858, 0.5999999999770569969, 1.000000000000000000),
 ( 0.2500000000000000000, 0.2499999999885285096, 0.2999999999827930308, 0.3999999999770569858, 0.5999999999770569969, 1.000000000000000000),
 ( 0.2500000000000000000, 0.2499999999885285096, 0.2999999999827930308, 0.3999999999770569858, 0.5999999999770569969, 1.000000000000000000) ) ) 
 REPRESENTATION_ITEM ( '' )  SURFACE ( )  );
#3596 = B_SPLINE_CURVE_WITH_KNOTS ( 'NONE', 3,
 ( #5948, #13202, #20475, #18692, #7840, #2512, #20950, #1321, #15704, #4873 ),
 .UNSPECIFIED., .F., .F.,
 ( 4, 2, 2, 2, 4 ),
 ( 0.000000000000000000, 0.2500000000000000000, 0.5000000000000000000, 0.7500000000000000000, 1.000000000000000000 ),
 .UNSPECIFIED. ) ;
#3597 = CARTESIAN_POINT ( 'NONE',  ( -24.99548980007219967, 37.05651868163716500, -148.5304149358840391 ) ) ;
#3598 = ORIENTED_EDGE ( 'NONE', *, *, #277, .F. ) ;
#3599 = CARTESIAN_POINT ( 'NONE',  ( -23.76507348488087956, 39.47303768213036079, -147.6024660352933893 ) ) ;
#3600 = CARTESIAN_POINT ( 'NONE',  ( -29.95440394289919794, 41.49361247766784544, -142.3913186430430073 ) ) ;
#3601 = DIRECTION ( 'NONE',  ( 0.9985681355238719137, -0.05349466063429310358, -4.511742413209420161E-12 ) ) ;
#3602 = CARTESIAN_POINT ( 'NONE',  ( 7.228461998321116688, 37.79745240714011345, -141.6854458089358104 ) ) ;
#3603 = ORIENTED_EDGE ( 'NONE', *, *, #18916, .F. ) ;
#3604 = CARTESIAN_POINT ( 'NONE',  ( -20.23971019809999916, 35.09018026569999904, -140.0771129649999978 ) ) ;
#3605 = CARTESIAN_POINT ( 'NONE',  ( -9.605700179776247793, 38.47911542068607105, -147.2779594871227857 ) ) ;
#3606 = CARTESIAN_POINT ( 'NONE',  ( -12.87073128380000142, -1.500000000000000000, -149.4704070610000031 ) ) ;
#3607 = ORIENTED_EDGE ( 'NONE', *, *, #10334, .T. ) ;
#3608 = DIRECTION ( 'NONE',  ( 0.000000000000000000, 0.000000000000000000, 1.000000000000000000 ) ) ;
#3609 = FILL_AREA_STYLE_COLOUR ( '', #16458 ) ;
#3610 = B_SPLINE_CURVE_WITH_KNOTS ( 'NONE', 5,
 ( #5925, #21788, #5473, #3685, #16529, #7371, #14630, #21898, #20570, #19013, #2490, #11977 ),
 .UNSPECIFIED., .F., .F.,
 ( 6, 3, 3, 6 ),
 ( 0.000000000000000000, 4.463483057499999518, 8.880954762089999122, 13.25426345570000031 ),
 .UNSPECIFIED. ) ;
#3611 = ADVANCED_FACE ( 'NONE', ( #11997 ), #11879, .T. ) ;
#3612 = VERTEX_POINT ( 'NONE', #19261 ) ;
#3613 = PLANE ( 'NONE',  #19072 ) ;
#3614 = CARTESIAN_POINT ( 'NONE',  ( -24.06602356359999817, 36.94557182220000158, -148.2530914610000252 ) ) ;
#3615 = LINE ( 'NONE', #2075, #16874 ) ;
#3616 = ORIENTED_EDGE ( 'NONE', *, *, #980, .F. ) ;
#3617 = DIRECTION ( 'NONE',  ( -1.000000000000000000, 0.000000000000000000, 2.257171095940000041E-12 ) ) ;
#3618 = CARTESIAN_POINT ( 'NONE',  ( -9.334216945200001447, -17.19633444960000190, -146.5552959529999839 ) ) ;
#3619 = ORIENTED_EDGE ( 'NONE', *, *, #22626, .F. ) ;
#3620 = DIRECTION ( 'NONE',  ( -3.994014902950000436E-29, 1.000000000000000000, -4.148443855749999753E-27 ) ) ;
#3621 = CARTESIAN_POINT ( 'NONE',  ( -18.85469010170000459, 37.03971195569999963, -148.4264296979999926 ) ) ;
#3623 = AXIS2_PLACEMENT_3D ( 'NONE', #5109, #21895, #23434 ) ;
#3622 = CARTESIAN_POINT ( 'NONE',  ( -2.499999999940000439, 37.00000000000000000, -144.0552959529999839 ) ) ;
#3624 = CARTESIAN_POINT ( 'NONE',  ( -6.603585321229999749, -20.59801339440000234, -143.5552959529999839 ) ) ;
#3625 = CARTESIAN_POINT ( 'NONE',  ( 23.50000000000000000, -20.50000000000000000, -144.7152959530000089 ) ) ;
#3626 = CARTESIAN_POINT ( 'NONE',  ( -17.68978131335608950, 36.92028947728229582, -140.0842674915935504 ) ) ;
#3627 = CONTEXT_DEPENDENT_SHAPE_REPRESENTATION ( #22877, #10096 ) ;
#3628 = CARTESIAN_POINT ( 'NONE',  ( 20.50000000000000000, 22.50000000000000000, -137.0552959530000123 ) ) ;
#3629 = LINE ( 'NONE', #3864, #19188 ) ;
#3630 = CARTESIAN_POINT ( 'NONE',  ( 16.65421564080000039, -18.61497348660000029, -145.5552959529999839 ) ) ;
#3631 = ORIENTED_EDGE ( 'NONE', *, *, #14672, .F. ) ;
#3632 = VERTEX_POINT ( 'NONE', #19148 ) ;
#3633 =( LENGTH_UNIT ( ) NAMED_UNIT ( * ) SI_UNIT ( .MILLI., .METRE. ) );
#3634 = ADVANCED_FACE ( 'NONE', ( #4989 ), #4512, .T. ) ;
#3635 = ORIENTED_EDGE ( 'NONE', *, *, #14869, .T. ) ;
#3636 = AXIS2_PLACEMENT_3D ( 'NONE', #5525, #11100, #23494 ) ;
#3637 = CARTESIAN_POINT ( 'NONE',  ( -15.79202522179999946, 35.03772048769999969, -148.2850092029999871 ) ) ;
#3638 = CARTESIAN_POINT ( 'NONE',  ( -13.14072436392984322, 35.21943041104802319, -148.3635587296070071 ) ) ;
#3639 = CARTESIAN_POINT ( 'NONE',  ( 4.999999999879999990, -2.250000000000000000, -135.0552959530000123 ) ) ;
#3640 = CIRCLE ( 'NONE', #4773, 2.999999999999999112 ) ;
#3641 = LINE ( 'NONE', #10875, #21424 ) ;
#3642 = ORIENTED_EDGE ( 'NONE', *, *, #11610, .F. ) ;
#3643 = CARTESIAN_POINT ( 'NONE',  ( -7.500000000000000000, 25.50000000000000000, -150.0552959529999839 ) ) ;
#3644 = CARTESIAN_POINT ( 'NONE',  ( -19.88002610979284057, 33.21367146195343167, -143.9008389802610282 ) ) ;
#3645 = DIRECTION ( 'NONE',  ( 1.000000000000000000, 0.000000000000000000, -4.430318231639999944E-12 ) ) ;
#3646 = DIRECTION ( 'NONE',  ( -0.7633862853691524286, -0.6459422414661293299, 5.800915303671162679E-15 ) ) ;
#3647 = EDGE_LOOP ( 'NONE', ( #3064, #16595, #12746, #18365 ) ) ;
#3648 = DIRECTION ( 'NONE',  ( 2.257144641399999941E-12, 0.000000000000000000, 1.000000000000000000 ) ) ;
#3649 = ORIENTED_EDGE ( 'NONE', *, *, #744, .F. ) ;
#3650 = CARTESIAN_POINT ( 'NONE',  ( 8.844715317520215336, 35.53941187169878191, -142.0263608017556010 ) ) ;
#3651 = LINE ( 'NONE', #5657, #1368 ) ;
#3652 = VECTOR ( 'NONE', #15946, 1000.000000000000227 ) ;
#3653 = CARTESIAN_POINT ( 'NONE',  ( 4.499999999879999102, -3.500000000000000000, -136.0552959530000123 ) ) ;
#3654 = AXIS2_PLACEMENT_3D ( 'NONE', #17640, #11920, #8468 ) ;
#3655 = ORIENTED_EDGE ( 'NONE', *, *, #3663, .F. ) ;
#3656 = CARTESIAN_POINT ( 'NONE',  ( 32.00000000000000000, -33.03620104880000241, -137.0552959530000123 ) ) ;
#3657 = VERTEX_POINT ( 'NONE', #1073 ) ;
#3658 = PLANE ( 'NONE',  #10935 ) ;
#3659 = DIRECTION ( 'NONE',  ( -2.602084704489999637E-17, 1.000000000000000000, 4.426606872070000353E-37 ) ) ;
#3660 = ORIENTED_EDGE ( 'NONE', *, *, #13176, .T. ) ;
#3661 = CARTESIAN_POINT ( 'NONE',  ( -26.59168384020000175, 38.48554521319999822, -140.5676127940000129 ) ) ;
#3662 = EDGE_LOOP ( 'NONE', ( #16024, #12240, #17141 ) ) ;
#3663 = EDGE_CURVE ( 'NONE', #23456, #19736, #6295, .T. ) ;
#3664 = CARTESIAN_POINT ( 'NONE',  ( -22.10875017890000294, 36.18377167419999552, -148.1739623899999856 ) ) ;
#3665 = CARTESIAN_POINT ( 'NONE',  ( 13.68320006080000084, -21.50000000000000000, -148.5552959529999839 ) ) ;
#3666 = EDGE_CURVE ( 'NONE', #6279, #14794, #11753, .T. ) ;
#3667 = ORIENTED_EDGE ( 'NONE', *, *, #2515, .T. ) ;
#3668 = CARTESIAN_POINT ( 'NONE',  ( 0.000000000000000000, 0.000000000000000000, 0.000000000000000000 ) ) ;
#3669 = EDGE_LOOP ( 'NONE', ( #3751, #13052, #5832, #1710 ) ) ;
#3670 = CARTESIAN_POINT ( 'NONE',  ( -27.35038827430062014, 41.32943388969216159, -143.4915779297264748 ) ) ;
#3671 = AXIS2_PLACEMENT_3D ( 'NONE', #4699, #3264, #14213 ) ;
#3672 = CARTESIAN_POINT ( 'NONE',  ( 4.500000000009999113, -2.000000000000000000, -136.0552959530000123 ) ) ;
#3673 = ORIENTED_EDGE ( 'NONE', *, *, #18818, .F. ) ;
#3674 = CARTESIAN_POINT ( 'NONE',  ( 2.170391987449999505, -12.72823260819999902, -145.5552959529999839 ) ) ;
#3675 = LINE ( 'NONE', #3561, #9103 ) ;
#3676 = DIRECTION ( 'NONE',  ( 1.000000000000000000, 0.000000000000000000, -2.715621035259064790E-14 ) ) ;
#3677 = VERTEX_POINT ( 'NONE', #17482 ) ;
#3678 = CARTESIAN_POINT ( 'NONE',  ( 6.500000000140000012, 20.50000000000000000, -146.5552959529999839 ) ) ;
#3679 = DIRECTION ( 'NONE',  ( 0.000000000000000000, 1.000000000000000000, 0.000000000000000000 ) ) ;
#3680 = VERTEX_POINT ( 'NONE', #19031 ) ;
#3681 = DIRECTION ( 'NONE',  ( 1.000000000000000000, 0.000000000000000000, -2.257453483404485639E-12 ) ) ;
#3682 = EDGE_CURVE ( 'NONE', #11025, #19591, #20522, .T. ) ;
#3683 = CARTESIAN_POINT ( 'NONE',  ( 32.50000000000000000, -33.03620104880000241, -137.0552959530000123 ) ) ;
#3684 = CARTESIAN_POINT ( 'NONE',  ( -17.27864984452603991, 40.23496799366807863, -142.1532139957253946 ) ) ;
#3685 = CARTESIAN_POINT ( 'NONE',  ( -22.31464002779999944, 34.51618902799999944, -147.4864127260000259 ) ) ;
#3686 = AXIS2_PLACEMENT_3D ( 'NONE', #11944, #8724, #16003 ) ;
#3687 = ORIENTED_EDGE ( 'NONE', *, *, #2358, .F. ) ;
#3688 = CARTESIAN_POINT ( 'NONE',  ( 0.8488229453839356564, 15.54483228932016026, -136.0552959530018882 ) ) ;
#3689 = DIRECTION ( 'NONE',  ( 4.510170015240000199E-12, -1.314504061159999897E-13, 1.000000000000000000 ) ) ;
#3690 = DIRECTION ( 'NONE',  ( -0.9954742291034677226, 0.09503188512734457583, 4.503697062742119365E-12 ) ) ;
#3691 = DIRECTION ( 'NONE',  ( 0.000000000000000000, 5.873289694040000105E-29, -1.000000000000000000 ) ) ;
#3692 = CARTESIAN_POINT ( 'NONE',  ( -31.00000000000000000, -51.50000000000000000, -149.5552959529999839 ) ) ;
#3693 = CYLINDRICAL_SURFACE ( 'NONE', #3750, 1.500000000000001554 ) ;
#3694 = ADVANCED_FACE ( 'NONE', ( #4639 ), #20947, .T. ) ;
#3695 = EDGE_LOOP ( 'NONE', ( #4377, #20478, #21447, #5174 ) ) ;
#3696 = PLANE ( 'NONE',  #12169 ) ;
#3697 = CARTESIAN_POINT ( 'NONE',  ( 6.500000000159999125, 20.50000000000000000, -139.5552959529999839 ) ) ;
#3698 = CARTESIAN_POINT ( 'NONE',  ( -6.909346445852020402, 37.92300339049243973, -148.1333867873126167 ) ) ;
#3699 = CARTESIAN_POINT ( 'NONE',  ( 4.750000000030000002, -40.36803398869999882, -137.0552959530000123 ) ) ;
#3700 = AXIS2_PLACEMENT_3D ( 'NONE', #10858, #14454, #15765 ) ;
#3701 = ORIENTED_EDGE ( 'NONE', *, *, #849, .F. ) ;
#3702 = CARTESIAN_POINT ( 'NONE',  ( 9.708726552585108749, -20.76023149958701453, -148.5552959529999839 ) ) ;
#3703 = EDGE_CURVE ( 'NONE', #2014, #3173, #11377, .T. ) ;
#3704 = CARTESIAN_POINT ( 'NONE',  ( -31.50000000000000000, 12.00000000000000000, -144.0552959529999839 ) ) ;
#3705 = ORIENTED_EDGE ( 'NONE', *, *, #12699, .T. ) ;
#3706 = DIRECTION ( 'NONE',  ( 2.257171095940000041E-12, 1.003664318210000046E-28, 1.000000000000000000 ) ) ;
#3707 = VERTEX_POINT ( 'NONE', #19623 ) ;
#3708 = CARTESIAN_POINT ( 'NONE',  ( -24.50448663600032972, 36.99790949613869628, -147.3823814620264159 ) ) ;
#3709 = EDGE_CURVE ( 'NONE', #1015, #22590, #5100, .T. ) ;
#3710 = CARTESIAN_POINT ( 'NONE',  ( -29.69384575750991218, 38.86443117690002680, -140.7775166546643391 ) ) ;
#3711 = EDGE_CURVE ( 'NONE', #11278, #1062, #5569, .T. ) ;
#3712 = CARTESIAN_POINT ( 'NONE',  ( -21.73453520639999681, 32.91403690879999289, -144.3663112600000318 ) ) ;
#3713 = CARTESIAN_POINT ( 'NONE',  ( 7.365399142987872239, 37.98233957550490913, -141.7561022823591657 ) ) ;
#3714 = ORIENTED_EDGE ( 'NONE', *, *, #5932, .T. ) ;
#3715 = CARTESIAN_POINT ( 'NONE',  ( -10.78990953686118104, 36.10633245638514666, -139.4672549339003353 ) ) ;
#3716 = CARTESIAN_POINT ( 'NONE',  ( -19.35423020444331144, 32.65090734717338705, -141.7482459578876615 ) ) ;
#3717 = EDGE_CURVE ( 'NONE', #23501, #4187, #21774, .T. ) ;
#3718 = FACE_OUTER_BOUND ( 'NONE', #13500, .T. ) ;
#3719 = PLANE ( 'NONE',  #12985 ) ;
#3720 = EDGE_CURVE ( 'NONE', #1364, #12024, #17479, .T. ) ;
#3721 = DIRECTION ( 'NONE',  ( 1.000000000000000000, 0.000000000000000000, 2.257144641399999941E-12 ) ) ;
#3722 = ORIENTED_EDGE ( 'NONE', *, *, #2957, .T. ) ;
#3723 = PRESENTATION_LAYER_ASSIGNMENT (  '', '', ( #18914 ) ) ;
#3724 = PLANE ( 'NONE',  #18665 ) ;
#3725 = DIRECTION ( 'NONE',  ( 0.000000000000000000, -1.000000000000000000, 8.159623473500000156E-13 ) ) ;
#3726 = DIRECTION ( 'NONE',  ( 1.000000000000000000, 0.000000000000000000, -4.510774274160000731E-12 ) ) ;
#3727 = CARTESIAN_POINT ( 'NONE',  ( -4.500067286917269982, 22.89748944254629848, -136.0552959529898658 ) ) ;
#3728 = SHAPE_REPRESENTATION ( 'Slider', ( #5025 ), #19488 ) ;
#3729 = VERTEX_POINT ( 'NONE', #23310 ) ;
#3730 = CARTESIAN_POINT ( 'NONE',  ( -4.875412749849999727, 39.32116320210000282, -140.9191069839999955 ) ) ;
#3731 = ORIENTED_EDGE ( 'NONE', *, *, #50, .T. ) ;
#3732 = CARTESIAN_POINT ( 'NONE',  ( 3.780861691979999772, -4.816373842840000030, -136.0552959530000123 ) ) ;
#3733 = VECTOR ( 'NONE', #23240, 1000.000000000000000 ) ;
#3734 = PLANE ( 'NONE',  #3386 ) ;
#3735 = AXIS2_PLACEMENT_3D ( 'NONE', #8390, #21018, #19216 ) ;
#3736 = CARTESIAN_POINT ( 'NONE',  ( -14.08020845438083235, -44.20076496858382598, -150.0552959529999839 ) ) ;
#3737 = LINE ( 'NONE', #3624, #17874 ) ;
#3738 = ADVANCED_FACE ( 'NONE', ( #3204 ), #5459, .T. ) ;
#3739 = DIRECTION ( 'NONE',  ( 4.430233957459999899E-12, -6.110667527539999876E-13, 1.000000000000000000 ) ) ;
#3740 = EDGE_CURVE ( 'NONE', #3831, #10198, #19390, .T. ) ;
#3741 = DIRECTION ( 'NONE',  ( 0.000000000000000000, 1.000000000000000000, 0.000000000000000000 ) ) ;
#3742 = CONTEXT_DEPENDENT_SHAPE_REPRESENTATION ( #16026, #19213 ) ;
#3743 = LINE ( 'NONE', #10983, #16613 ) ;
#3744 = DIRECTION ( 'NONE',  ( -1.000000000000000000, 0.000000000000000000, 0.000000000000000000 ) ) ;
#3745 = CARTESIAN_POINT ( 'NONE',  ( 6.500000000140000012, 20.50000000000000000, -146.5552959529999839 ) ) ;
#3746 = VERTEX_POINT ( 'NONE', #7244 ) ;
#3747 = UNCERTAINTY_MEASURE_WITH_UNIT (LENGTH_MEASURE( 1.000000000000000082E-05 ), #1198, 'distance_accuracy_value', 'NONE');
#3748 = ORIENTED_EDGE ( 'NONE', *, *, #20592, .T. ) ;
#3749 = VECTOR ( 'NONE', #13637, 1000.000000000000227 ) ;
#3750 = AXIS2_PLACEMENT_3D ( 'NONE', #11052, #21795, #7139 ) ;
#3751 = ORIENTED_EDGE ( 'NONE', *, *, #21172, .T. ) ;
#3752 = CARTESIAN_POINT ( 'NONE',  ( -16.84295571282639870, 33.21673955036126813, -144.3448215146551661 ) ) ;
#3753 = CARTESIAN_POINT ( 'NONE',  ( 32.50000000000000000, 20.96379895120000114, -136.0552959530000123 ) ) ;
#3754 = VERTEX_POINT ( 'NONE', #3317 ) ;
#3755 = DIRECTION ( 'NONE',  ( 0.2451800884060535979, 0.9694775522152123681, -1.317373699560290683E-12 ) ) ;
#3756 = ORIENTED_EDGE ( 'NONE', *, *, #1371, .T. ) ;
#3757 = VECTOR ( 'NONE', #19748, 1000.000000000000000 ) ;
#3758 = CARTESIAN_POINT ( 'NONE',  ( 6.500000000149999124, 12.50000000000000000, -143.5552959529999839 ) ) ;
#3759 = CARTESIAN_POINT ( 'NONE',  ( -19.91220883949999987, 32.96944242089999477, -141.9853941000000077 ) ) ;
#3760 = CARTESIAN_POINT ( 'NONE',  ( -3.499999999959999997, 46.50000000000000000, -136.0552959530000123 ) ) ;
#3761 = ORIENTED_EDGE ( 'NONE', *, *, #3502, .F. ) ;
#3762 = CARTESIAN_POINT ( 'NONE',  ( 1.000000000160000013, 36.50000000000000000, -140.0552959529999839 ) ) ;
#3763 = ORIENTED_EDGE ( 'NONE', *, *, #6126, .F. ) ;
#3764 = CARTESIAN_POINT ( 'NONE',  ( 9.556107899309107978, 35.93480091585412595, -141.7935801463470966 ) ) ;
#3765 = AXIS2_PLACEMENT_3D ( 'NONE', #11756, #1080, #2748 ) ;
#3766 = EDGE_CURVE ( 'NONE', #2602, #2360, #1929, .T. ) ;
#3767 = DIRECTION ( 'NONE',  ( -2.508215857230000030E-12, 0.000000000000000000, 1.000000000000000000 ) ) ;
#3768 = AXIS2_PLACEMENT_3D ( 'NONE', #1000, #22644, #13718 ) ;
#3769 = EDGE_CURVE ( 'NONE', #7769, #20668, #5344, .T. ) ;
#3770 = DIRECTION ( 'NONE',  ( 7.105427352750000330E-15, -1.000000000000000000, -1.603797727410000024E-26 ) ) ;
#3771 = ORIENTED_EDGE ( 'NONE', *, *, #21036, .F. ) ;
#3772 = AXIS2_PLACEMENT_3D ( 'NONE', #8330, #3340, #10577 ) ;
#3773 = VECTOR ( 'NONE', #3539, 1000.000000000000000 ) ;
#3774 = DIRECTION ( 'NONE',  ( 1.000000000000000000, 0.000000000000000000, 0.000000000000000000 ) ) ;
#3775 = ORIENTED_EDGE ( 'NONE', *, *, #16484, .T. ) ;
#3776 = SURFACE_STYLE_USAGE ( .BOTH. , #16850 ) ;
#3777 = CARTESIAN_POINT ( 'NONE',  ( -24.97797643630000053, 37.05442817780000553, -147.8575004449999994 ) ) ;
#3778 = ORIENTED_EDGE ( 'NONE', *, *, #11258, .T. ) ;
#3779 = CARTESIAN_POINT ( 'NONE',  ( -26.25246229356530492, 40.09452554318689010, -142.2796191593848221 ) ) ;
#3780 = EDGE_LOOP ( 'NONE', ( #4972, #20052 ) ) ;
#3781 = CARTESIAN_POINT ( 'NONE',  ( -23.02519999780000148, 33.35976406540000028, -141.9520978260000277 ) ) ;
#3782 = CARTESIAN_POINT ( 'NONE',  ( -3.765581077008664401, 46.50000000000002842, -136.0552959529915142 ) ) ;
#3783 = ORIENTED_EDGE ( 'NONE', *, *, #8938, .F. ) ;
#3784 = PRODUCT_CONTEXT ( 'NONE', #9918, 'mechanical' ) ;
#3785 = PRODUCT_DEFINITION_SHAPE ( 'NONE', 'NONE',  #19394 ) ;
#3786 = VECTOR ( 'NONE', #19370, 1000.000000000000000 ) ;
#3787 = ORIENTED_EDGE ( 'NONE', *, *, #2432, .F. ) ;
#3788 = CARTESIAN_POINT ( 'NONE',  ( -26.61707828802655484, 36.92896776167479089, -139.7487649555727103 ) ) ;
#3789 = VECTOR ( 'NONE', #16063, 1000.000000000000000 ) ;
#3790 = CARTESIAN_POINT ( 'NONE',  ( 6.499999999879999102, -3.500000000000000000, -135.4552959529999896 ) ) ;
#3791 = LINE ( 'NONE', #219, #16054 ) ;
#3792 = CARTESIAN_POINT ( 'NONE',  ( 13.13369214870000157, 51.50000000000000000, -137.0552959530000123 ) ) ;
#3793 = AXIS2_PLACEMENT_3D ( 'NONE', #17478, #19145, #2848 ) ;
#3794 = CARTESIAN_POINT ( 'NONE',  ( 32.50000000000000000, 0.000000000000000000, -136.0552959530000123 ) ) ;
#3795 = AXIS2_PLACEMENT_3D ( 'NONE', #22433, #13384, #20652 ) ;
#3796 = DIRECTION ( 'NONE',  ( 0.000000000000000000, 1.000000000000000000, 0.000000000000000000 ) ) ;
#3797 = VERTEX_POINT ( 'NONE', #10907 ) ;
#3798 = CARTESIAN_POINT ( 'NONE',  ( -16.54277457359999914, 34.95491693750000195, -141.0331736029999945 ) ) ;
#3799 = ADVANCED_FACE ( 'NONE', ( #10438 ), #19744, .T. ) ;
#3800 = DIRECTION ( 'NONE',  ( 4.430233957459999899E-12, -6.110667527539999876E-13, 1.000000000000000000 ) ) ;
#3801 = EDGE_CURVE ( 'NONE', #17690, #3040, #15927, .T. ) ;
#3802 = ORIENTED_EDGE ( 'NONE', *, *, #9650, .F. ) ;
#3803 = CARTESIAN_POINT ( 'NONE',  ( 4.109450702737304617, -4.961822747171590997, -150.0552959529999839 ) ) ;
#3804 = FACE_OUTER_BOUND ( 'NONE', #15803, .T. ) ;
#3805 = CARTESIAN_POINT ( 'NONE',  ( -17.22605506639999717, 36.97564272059999979, -139.5994799229999899 ) ) ;
#3806 = CARTESIAN_POINT ( 'NONE',  ( -29.16261562813939179, 41.45297187880490952, -142.5000714354081595 ) ) ;
#3807 = ORIENTED_EDGE ( 'NONE', *, *, #13030, .T. ) ;
#3808 = CARTESIAN_POINT ( 'NONE',  ( -8.565647946148805758, 36.93510680655035827, -139.7232782065093488 ) ) ;
#3809 = DIRECTION ( 'NONE',  ( -1.000000000000000000, 0.000000000000000000, 1.701177084980000217E-20 ) ) ;
#3810 = VECTOR ( 'NONE', #7889, 1000.000000000000000 ) ;
#3811 = AXIS2_PLACEMENT_3D ( 'NONE', #23132, #5151, #12400 ) ;
#3812 = FACE_BOUND ( 'NONE', #21940, .T. ) ;
#3813 = DIRECTION ( 'NONE',  ( 2.602084747549999882E-17, -1.000000000000000000, -5.873289694040000105E-29 ) ) ;
#3814 = DIRECTION ( 'NONE',  ( 8.955190032050000935E-12, -9.104778821549999739E-13, 1.000000000000000000 ) ) ;
#3815 = AXIS2_PLACEMENT_3D ( 'NONE', #10620, #1497, #12184 ) ;
#3816 = DIRECTION ( 'NONE',  ( 8.955190032050000935E-12, -9.104778821549999739E-13, 1.000000000000000000 ) ) ;
#3817 = AXIS2_PLACEMENT_3D ( 'NONE', #9004, #12818, #18419 ) ;
#3818 = ORIENTED_EDGE ( 'NONE', *, *, #9759, .F. ) ;
#3819 = CARTESIAN_POINT ( 'NONE',  ( -26.86963863710373701, 36.92213009831746007, -147.8538433455846359 ) ) ;
#3820 = CARTESIAN_POINT ( 'NONE',  ( -13.86630785140000022, -50.50000000000000000, -143.0552959529999839 ) ) ;
#3821 = DIRECTION ( 'NONE',  ( -1.769477252542410170E-11, 0.000000000000000000, 1.000000000000000000 ) ) ;
#3822 = CARTESIAN_POINT ( 'NONE',  ( -4.780317782130000914, 38.61135856239999953, -140.5115181619999873 ) ) ;
#3823 = CARTESIAN_POINT ( 'NONE',  ( -13.53904098499752884, -43.39262182653893518, -136.0552959530033377 ) ) ;
#3824 = ORIENTED_EDGE ( 'NONE', *, *, #18377, .T. ) ;
#3825 = LINE ( 'NONE', #7274, #2625 ) ;
#3826 = DIRECTION ( 'NONE',  ( 0.000000000000000000, -1.000000000000000000, 8.159623473500000156E-13 ) ) ;
#3827 = ORIENTED_EDGE ( 'NONE', *, *, #14838, .T. ) ;
#3828 = VECTOR ( 'NONE', #5477, 1000.000000000000000 ) ;
#3829 = AXIS2_PLACEMENT_3D ( 'NONE', #7095, #1874, #16382 ) ;
#3830 = ADVANCED_FACE ( 'NONE', ( #17834 ), #14508, .F. ) ;
#3831 = VERTEX_POINT ( 'NONE', #19972 ) ;
#3832 = LINE ( 'NONE', #261, #17726 ) ;
#3833 = DIRECTION ( 'NONE',  ( -1.000000000000000000, 0.000000000000000000, 0.000000000000000000 ) ) ;
#3834 = CARTESIAN_POINT ( 'NONE',  ( -33.42928932190000069, -65.97217712079999785, -146.7500980969999773 ) ) ;
#3835 = CYLINDRICAL_SURFACE ( 'NONE', #12518, 5.999999999999999112 ) ;
#3836 = VERTEX_POINT ( 'NONE', #8891 ) ;
#3837 = CARTESIAN_POINT ( 'NONE',  ( 24.59017985859999911, -26.91621017459999976, -147.5552959529999839 ) ) ;
#3838 = CARTESIAN_POINT ( 'NONE',  ( -19.33242029388426531, 35.08629375165114084, -139.8117605349705173 ) ) ;
#3839 = CARTESIAN_POINT ( 'NONE',  ( -4.499999999949999996, 34.00000000000000000, -150.0552959529999839 ) ) ;
#3840 = FACE_OUTER_BOUND ( 'NONE', #10713, .T. ) ;
#3841 = FACE_OUTER_BOUND ( 'NONE', #20320, .T. ) ;
#3842 = EDGE_CURVE ( 'NONE', #2622, #1486, #16287, .T. ) ;
#3843 = VECTOR ( 'NONE', #20387, 1000.000000000000000 ) ;
#3844 = CARTESIAN_POINT ( 'NONE',  ( 17.49993271309341125, 22.89748944248912466, -136.0552959530394617 ) ) ;
#3845 = ADVANCED_BREP_SHAPE_REPRESENTATION ( '', ( #19750, #5025 ), #9222 ) ;
#3846 = DIRECTION ( 'NONE',  ( -0.6459422414661291079, -0.7633862853691523176, -2.273736754430455399E-12 ) ) ;
#3847 = DIRECTION ( 'NONE',  ( 2.256861364460000137E-12, 0.000000000000000000, 1.000000000000000000 ) ) ;
#3848 = CARTESIAN_POINT ( 'NONE',  ( 4.750000000000000000, -47.00000000000000000, -150.5552959529999839 ) ) ;
#3849 = EDGE_CURVE ( 'NONE', #17357, #22329, #1428, .T. ) ;
#3850 = ORIENTED_EDGE ( 'NONE', *, *, #225, .F. ) ;
#3851 = CARTESIAN_POINT ( 'NONE',  ( -6.093288228365016934, 36.94882630176445559, -147.6373263597673997 ) ) ;
#3852 = EDGE_LOOP ( 'NONE', ( #16503, #2413, #5372, #21942 ) ) ;
#3853 = LINE ( 'NONE', #4321, #2708 ) ;
#3854 = EDGE_CURVE ( 'NONE', #2360, #2602, #14067, .T. ) ;
#3855 = CARTESIAN_POINT ( 'NONE',  ( -6.049191701419999845, -14.51144913589999952, -146.5552959529999839 ) ) ;
#3856 = CARTESIAN_POINT ( 'NONE',  ( -9.999999999969999109, 42.50000000000000000, -137.0552959530000123 ) ) ;
#3857 = VECTOR ( 'NONE', #3299, 1000.000000000000000 ) ;
#3858 = CARTESIAN_POINT ( 'NONE',  ( -38.39535039439999764, 45.00000000000000000, -147.5552959529999839 ) ) ;
#3859 = VECTOR ( 'NONE', #9637, 1000.000000000000000 ) ;
#3860 = CARTESIAN_POINT ( 'NONE',  ( -12.85940537543597806, 33.96382169714053845, -145.9084692328443964 ) ) ;
#3861 = DIRECTION ( 'NONE',  ( 0.000000000000000000, -1.000000000000000000, 0.000000000000000000 ) ) ;
#3862 = DIRECTION ( 'NONE',  ( 0.000000000000000000, 0.000000000000000000, -1.000000000000000000 ) ) ;
#3863 = LINE ( 'NONE', #5286, #18515 ) ;
#3864 = CARTESIAN_POINT ( 'NONE',  ( 1.133692148650000009, 50.50000000000000000, -136.5552959530000123 ) ) ;
#3865 = LINE ( 'NONE', #7424, #16629 ) ;
#3866 = EDGE_CURVE ( 'NONE', #8499, #17090, #9864, .T. ) ;
#3867 = ORIENTED_EDGE ( 'NONE', *, *, #14460, .T. ) ;
#3868 = EDGE_CURVE ( 'NONE', #15515, #5708, #21295, .T. ) ;
#3869 =( BOUNDED_CURVE ( )  B_SPLINE_CURVE ( 5, ( #22580, #19121, #2826, #9944, #13776, #12088, #1296, #2946, #13996, #10305, #1179, #4967 ),
 .UNSPECIFIED., .F., .F. ) 
 B_SPLINE_CURVE_WITH_KNOTS ( ( 6, 3, 3, 6 ),
 ( 0.000000000000000000, 4.564346237179999655, 9.066392868600001265, 13.51003987140000007 ),
 .UNSPECIFIED. ) 
 CURVE ( )  GEOMETRIC_REPRESENTATION_ITEM ( )  RATIONAL_B_SPLINE_CURVE ( ( 0.2500000000000000000, 0.2500000000000000000, 0.2500000000000000000, 0.2500000000000000000, 0.2500000000000000000, 0.2500000000000000000, 0.2500000000000000000, 0.2500000000000000000, 0.2500000000000000000, 0.2500000000000000000, 0.2500000000000000000, 0.2500000000000000000 ) ) 
 REPRESENTATION_ITEM ( '' )  );
#3870 = VERTEX_POINT ( 'NONE', #22336 ) ;
#3871 =( NAMED_UNIT ( * ) PLANE_ANGLE_UNIT ( ) SI_UNIT ( $, .RADIAN. ) );
#3872 = ORIENTED_EDGE ( 'NONE', *, *, #9924, .T. ) ;
#3873 = CARTESIAN_POINT ( 'NONE',  ( -13.03986231551754749, 36.13583152158137324, -148.5880302933537678 ) ) ;
#3874 = CARTESIAN_POINT ( 'NONE',  ( 31.00000000000000000, 39.80430157320000006, -149.5552959529999839 ) ) ;
#3875 = AXIS2_PLACEMENT_3D ( 'NONE', #17145, #22619, #18089 ) ;
#3876 = CIRCLE ( 'NONE', #3116, 2.999999999999999112 ) ;
#3877 = CARTESIAN_POINT ( 'NONE',  ( 23.08797222880000177, -15.45109671570000032, -143.5552959529999839 ) ) ;
#3878 = VECTOR ( 'NONE', #18845, 1000.000000000000000 ) ;
#3879 = B_SPLINE_CURVE_WITH_KNOTS ( 'NONE', 5,
 ( #6996, #12456, #3429, #16280, #20209, #12929, #7686, #11024, #16735 ),
 .UNSPECIFIED., .F., .F.,
 ( 6, 3, 6 ),
 ( 0.000000000000000000, 5.731822293570000504, 9.005131590149998644 ),
 .UNSPECIFIED. ) ;
#3880 = ADVANCED_FACE ( 'NONE', ( #4022 ), #572, .F. ) ;
#3881 = VERTEX_POINT ( 'NONE', #5913 ) ;
#3882 = CARTESIAN_POINT ( 'NONE',  ( 24.01497134763214802, 33.88109793996618890, -136.0552959530542125 ) ) ;
#3883 = CARTESIAN_POINT ( 'NONE',  ( -19.48816230390420046, 36.23023348065551374, -140.2952556283244121 ) ) ;
#3884 = EDGE_CURVE ( 'NONE', #12276, #23083, #2368, .T. ) ;
#3885 = DIRECTION ( 'NONE',  ( 0.000000000000000000, 0.000000000000000000, 1.000000000000000000 ) ) ;
#3886 = EDGE_LOOP ( 'NONE', ( #1726, #4484, #8733, #18407, #18045 ) ) ;
#3887 = CARTESIAN_POINT ( 'NONE',  ( -20.45144833149999997, 36.94873838139999833, -139.8044047869999815 ) ) ;
#3888 = EDGE_CURVE ( 'NONE', #8429, #10865, #16744, .T. ) ;
#3889 = EDGE_CURVE ( 'NONE', #565, #13650, #5798, .T. ) ;
#3890 = CARTESIAN_POINT ( 'NONE',  ( 8.879708087000684813, 38.45148868343596860, -142.0197959584526188 ) ) ;
#3891 = CARTESIAN_POINT ( 'NONE',  ( 8.750000000030000891, -39.98606797749999942, -136.5552959530000123 ) ) ;
#3892 = FACE_OUTER_BOUND ( 'NONE', #11757, .T. ) ;
#3893 = ORIENTED_EDGE ( 'NONE', *, *, #14106, .T. ) ;
#3894 = VECTOR ( 'NONE', #2879, 1000.000000000000000 ) ;
#3895 = VECTOR ( 'NONE', #17954, 1000.000000000000114 ) ;
#3896 = CARTESIAN_POINT ( 'NONE',  ( -26.39607007120000048, 36.95534867429999792, -140.3840478969999879 ) ) ;
#3897 = ORIENTED_EDGE ( 'NONE', *, *, #22589, .T. ) ;
#3898 = DIRECTION ( 'NONE',  ( 1.000000000000000000, 2.688820921349999492E-17, 0.000000000000000000 ) ) ;
#3899 = VERTEX_POINT ( 'NONE', #6151 ) ;
#3900 = CARTESIAN_POINT ( 'NONE',  ( -25.84964047065839665, 38.84307078620516052, -139.9757795271566181 ) ) ;
#3901 = VERTEX_POINT ( 'NONE', #3792 ) ;
#3902 = CARTESIAN_POINT ( 'NONE',  ( -21.81749540767824769, 32.51398808010975472, -143.4422501083998611 ) ) ;
#3903 = ORIENTED_EDGE ( 'NONE', *, *, #12855, .T. ) ;
#3904 = LINE ( 'NONE', #682, #19720 ) ;
#3905 = VERTEX_POINT ( 'NONE', #15199 ) ;
#3906 = VERTEX_POINT ( 'NONE', #457 ) ;
#3907 = CARTESIAN_POINT ( 'NONE',  ( -26.95224972436776056, 39.68365438087440111, -147.7577323693793971 ) ) ;
#3908 = DIRECTION ( 'NONE',  ( 1.527666881879999979E-13, 8.171241461240000022E-13, 1.000000000000000000 ) ) ;
#3909 = EDGE_CURVE ( 'NONE', #13656, #18172, #15901, .T. ) ;
#3910 = CARTESIAN_POINT ( 'NONE',  ( 12.46241645105735607, 25.07592078380848477, -150.0552959529999839 ) ) ;
#3911 =( GEOMETRIC_REPRESENTATION_CONTEXT ( 3 ) GLOBAL_UNCERTAINTY_ASSIGNED_CONTEXT ( ( #7317 ) ) GLOBAL_UNIT_ASSIGNED_CONTEXT ( ( #15284, #1005, #9776 ) ) REPRESENTATION_CONTEXT ( 'NONE', 'WORKASPACE' ) );
#3912 = DIRECTION ( 'NONE',  ( 2.256988247090000272E-12, 0.000000000000000000, 1.000000000000000000 ) ) ;
#3913 = AXIS2_PLACEMENT_3D ( 'NONE', #8565, #15837, #23103 ) ;
#3914 = PLANE ( 'NONE',  #10248 ) ;
#3915 = CARTESIAN_POINT ( 'NONE',  ( -8.271665395864435055, 36.97019838859878149, -139.4157638768422203 ) ) ;
#3916 = VERTEX_POINT ( 'NONE', #21991 ) ;
#3917 = CARTESIAN_POINT ( 'NONE',  ( 32.50000000000000000, -21.03620104879999886, -136.0552959530000123 ) ) ;
#3918 = CARTESIAN_POINT ( 'NONE',  ( 13.13369214870000157, -51.00000000000000000, -136.0552959530000123 ) ) ;
#3919 = ORIENTED_EDGE ( 'NONE', *, *, #849, .T. ) ;
#3920 = DIRECTION ( 'NONE',  ( -0.09606172499277226828, -0.9953753789357124848, 8.268133652477615271E-13 ) ) ;
#3921 = CARTESIAN_POINT ( 'NONE',  ( -12.06588019170748183, 41.72429084328257431, -143.6635755491118402 ) ) ;
#3922 = CARTESIAN_POINT ( 'NONE',  ( -17.20598434367817120, 40.91627233628883431, -144.4696775178145174 ) ) ;
#3923 = CARTESIAN_POINT ( 'NONE',  ( -29.28558960869785466, 40.89060929661447119, -145.6601555479529111 ) ) ;
#3924 = ORIENTED_EDGE ( 'NONE', *, *, #1718, .F. ) ;
#3925 = SURFACE_STYLE_FILL_AREA ( #20232 ) ;
#3926 = CARTESIAN_POINT ( 'NONE',  ( -26.39607007120000048, 36.95534867429999792, -140.3840478969999879 ) ) ;
#3927 = ORIENTED_EDGE ( 'NONE', *, *, #19204, .F. ) ;
#3928 = DIRECTION ( 'NONE',  ( 1.000000000000000000, 0.000000000000000000, 0.000000000000000000 ) ) ;
#3929 = PLANE ( 'NONE',  #18704 ) ;
#3930 = CARTESIAN_POINT ( 'NONE',  ( 31.50000000000000000, 20.96379895120000114, -137.0552959530000123 ) ) ;
#3931 = CARTESIAN_POINT ( 'NONE',  ( -20.08037650824895692, 40.50744741020064055, -142.1449807696999983 ) ) ;
#3932 = VERTEX_POINT ( 'NONE', #220 ) ;
#3933 = DIRECTION ( 'NONE',  ( -0.1736481776649230480, 0.000000000000000000, 0.9848077530125620704 ) ) ;
#3934 = CARTESIAN_POINT ( 'NONE',  ( 20.50000000000000000, 25.50000000000000000, -150.0552959529999839 ) ) ;
#3935 = ADVANCED_FACE ( 'NONE', ( #7919 ), #20090, .F. ) ;
#3936 = CARTESIAN_POINT ( 'NONE',  ( -12.58047663530000015, 34.35960099889999952, -147.8017659109999897 ) ) ;
#3937 = CARTESIAN_POINT ( 'NONE',  ( -10.49999999989999822, 39.50000000000000000, -144.0552959529999839 ) ) ;
#3938 = EDGE_CURVE ( 'NONE', #9007, #12574, #4130, .T. ) ;
#3939 = CARTESIAN_POINT ( 'NONE',  ( -35.07300000000000040, 11.44852983560000048, -144.5552959529999839 ) ) ;
#3940 = ORIENTED_EDGE ( 'NONE', *, *, #14964, .F. ) ;
#3941 = LINE ( 'NONE', #9383, #5278 ) ;
#3942 = DIRECTION ( 'NONE',  ( 1.000000000000000000, 0.000000000000000000, -2.253752739989067373E-12 ) ) ;
#3943 = PRODUCT_DEFINITION_FORMATION_WITH_SPECIFIED_SOURCE ( 'ANY', '', #5209, .NOT_KNOWN. ) ;
#3944 = ORIENTED_EDGE ( 'NONE', *, *, #15067, .F. ) ;
#3945 = VECTOR ( 'NONE', #16254, 1000.000000000000000 ) ;
#3946 = ORIENTED_EDGE ( 'NONE', *, *, #12869, .F. ) ;
#3947 = CARTESIAN_POINT ( 'NONE',  ( -22.10824191589185972, -32.00000000000000000, -149.4708568729777483 ) ) ;
#3948 = EDGE_CURVE ( 'NONE', #15229, #22408, #13537, .T. ) ;
#3949 = CARTESIAN_POINT ( 'NONE',  ( 12.18320006080000084, -19.50000000000000000, -148.5552959529999839 ) ) ;
#3950 = CARTESIAN_POINT ( 'NONE',  ( 15.59498359470000040, -26.23371093219999750, -147.5552959529999839 ) ) ;
#3951 = DIRECTION ( 'NONE',  ( -2.252420472359999842E-12, 0.000000000000000000, 1.000000000000000000 ) ) ;
#3952 = ORIENTED_EDGE ( 'NONE', *, *, #15367, .F. ) ;
#3953 = LINE ( 'NONE', #11532, #13181 ) ;
#3954 = CARTESIAN_POINT ( 'NONE',  ( -20.07061698099752789, 34.98295635200901188, -139.7991296525235043 ) ) ;
#3955 = CARTESIAN_POINT ( 'NONE',  ( 24.11847952820000174, -31.58456057200000089, -142.5552959529999839 ) ) ;
#3956 = CARTESIAN_POINT ( 'NONE',  ( -46.50000000000000000, 26.50000000000000000, -148.4460207619999892 ) ) ;
#3957 = CARTESIAN_POINT ( 'NONE',  ( -24.89658049647220039, 37.98069042798901052, -148.5190484855092166 ) ) ;
#3958 = CARTESIAN_POINT ( 'NONE',  ( -42.28007584270000052, 29.00000000000000000, -143.7573642109999810 ) ) ;
#3959 = EDGE_CURVE ( 'NONE', #23250, #15992, #333, .T. ) ;
#3960 = VECTOR ( 'NONE', #15134, 1000.000000000000227 ) ;
#3961 = LINE ( 'NONE', #1337, #23256 ) ;
#3962 = CARTESIAN_POINT ( 'NONE',  ( 13.13369214870000157, 51.50000000000000000, -136.5552959530000123 ) ) ;
#3963 = EDGE_CURVE ( 'NONE', #7923, #13663, #18767, .T. ) ;
#3964 = CARTESIAN_POINT ( 'NONE',  ( 1.342750202250000191, -63.28208324180000233, -144.0552959529999839 ) ) ;
#3965 = ORIENTED_EDGE ( 'NONE', *, *, #7207, .F. ) ;
#3966 = CARTESIAN_POINT ( 'NONE',  ( -5.288267155659133856, 38.37431289982901461, -140.9004779445601798 ) ) ;
#3967 = ORIENTED_EDGE ( 'NONE', *, *, #18531, .T. ) ;
#3968 = DIRECTION ( 'NONE',  ( 0.7071067811870332953, 0.000000000000000000, 0.7071067811860618502 ) ) ;
#3969 = CARTESIAN_POINT ( 'NONE',  ( -22.72559961389999827, 32.84666773589999877, -144.4841142160000231 ) ) ;
#3970 = CARTESIAN_POINT ( 'NONE',  ( 21.44117969379999877, -21.36894679869999791, -146.5552959529999839 ) ) ;
#3971 = ORIENTED_EDGE ( 'NONE', *, *, #4430, .T. ) ;
#3972 = CARTESIAN_POINT ( 'NONE',  ( -12.05141338350562563, 35.34196401310663305, -147.7430715653573827 ) ) ;
#3973 = LINE ( 'NONE', #9418, #11219 ) ;
#3974 = AXIS2_PLACEMENT_3D ( 'NONE', #14177, #18219, #21442 ) ;
#3975 = DIRECTION ( 'NONE',  ( 0.9953753789357124848, -0.09606172499277225441, -7.355811845627870223E-14 ) ) ;
#3976 = LINE ( 'NONE', #18731, #21949 ) ;
#3977 = DIRECTION ( 'NONE',  ( 0.000000000000000000, 1.000000000000000000, 0.000000000000000000 ) ) ;
#3978 = EDGE_CURVE ( 'NONE', #18478, #16896, #20329, .T. ) ;
#3979 = PLANE ( 'NONE',  #21218 ) ;
#3980 = ORIENTED_EDGE ( 'NONE', *, *, #17641, .F. ) ;
#3981 = CARTESIAN_POINT ( 'NONE',  ( -4.500000000000000000, 34.00000000000000000, -150.5552959529999839 ) ) ;
#3982 = ORIENTED_EDGE ( 'NONE', *, *, #17873, .T. ) ;
#3983 = ORIENTED_EDGE ( 'NONE', *, *, #9951, .F. ) ;
#3984 = CARTESIAN_POINT ( 'NONE',  ( -13.27736068057458141, 36.23365056575769216, -148.2500542414416600 ) ) ;
#3985 = LINE ( 'NONE', #11218, #16794 ) ;
#3986 = EDGE_CURVE ( 'NONE', #18032, #5950, #9699, .T. ) ;
#3987 = CARTESIAN_POINT ( 'NONE',  ( 7.480639893073429469, 27.95196862336259258, -136.0552959530169232 ) ) ;
#3988 = ORIENTED_EDGE ( 'NONE', *, *, #13351, .T. ) ;
#3989 = CARTESIAN_POINT ( 'NONE',  ( 23.49999999970000175, -20.50000000000000000, -148.5552959529999839 ) ) ;
#3990 = CARTESIAN_POINT ( 'NONE',  ( -13.86630785130000021, 50.50000000000000000, -136.0552959530000123 ) ) ;
#3991 = VECTOR ( 'NONE', #18606, 1000.000000000000000 ) ;
#3992 = DIRECTION ( 'NONE',  ( 2.602084747549999882E-17, -1.000000000000000000, -5.873289694040000105E-29 ) ) ;
#3993 = ORIENTED_EDGE ( 'NONE', *, *, #11131, .F. ) ;
#3994 = CARTESIAN_POINT ( 'NONE',  ( -21.27630696881890771, 40.59564883395965751, -144.4447941612343982 ) ) ;
#3995 = EDGE_CURVE ( 'NONE', #6018, #5559, #689, .T. ) ;
#3996 = CARTESIAN_POINT ( 'NONE',  ( 9.990807518853022984, 37.19361385680454646, -141.5610522423011730 ) ) ;
#3997 = EDGE_CURVE ( 'NONE', #14626, #8533, #16513, .T. ) ;
#3998 = DIRECTION ( 'NONE',  ( 0.000000000000000000, -1.000000000000000000, 0.000000000000000000 ) ) ;
#3999 = CARTESIAN_POINT ( 'NONE',  ( -32.50000000000000000, 50.00000000000000000, -149.5552959529999839 ) ) ;
#4000 = EDGE_LOOP ( 'NONE', ( #5638, #20070, #4641, #8074 ) ) ;
#4001 =( BOUNDED_CURVE ( )  B_SPLINE_CURVE ( 5, ( #23158, #8618, #13878, #15893, #13991, #17575, #10518, #1288, #19593, #1519, #4837, #20912 ),
 .UNSPECIFIED., .F., .F. ) 
 B_SPLINE_CURVE_WITH_KNOTS ( ( 6, 3, 3, 6 ),
 ( 0.000000000000000000, 4.371092480729999785, 8.745625541600000830, 13.12578902609999965 ),
 .UNSPECIFIED. ) 
 CURVE ( )  GEOMETRIC_REPRESENTATION_ITEM ( )  RATIONAL_B_SPLINE_CURVE ( ( 0.2500000000000000000, 0.2500000000000000000, 0.2500000000000000000, 0.2500000000000000000, 0.2500000000000000000, 0.2500000000000000000, 0.2500000000000000000, 0.2500000000000000000, 0.2500000000000000000, 0.2500000000000000000, 0.2500000000000000000, 0.2500000000000000000 ) ) 
 REPRESENTATION_ITEM ( '' )  );
#4002 = ADVANCED_FACE ( 'NONE', ( #2128 ), #9349, .T. ) ;
#4003 = EDGE_CURVE ( 'NONE', #4587, #11453, #6379, .T. ) ;
#4004 = CARTESIAN_POINT ( 'NONE',  ( 8.250000000000000000, -42.23606797749999942, -151.0552959529999839 ) ) ;
#4005 = ORIENTED_EDGE ( 'NONE', *, *, #4979, .F. ) ;
#4006 = VECTOR ( 'NONE', #16698, 1000.000000000000000 ) ;
#4007 = CARTESIAN_POINT ( 'NONE',  ( 7.750000000000000000, -41.23606797749999942, -151.0552959529999839 ) ) ;
#4008 = EDGE_CURVE ( 'NONE', #2494, #9931, #13517, .T. ) ;
#4009 = ORIENTED_EDGE ( 'NONE', *, *, #23226, .F. ) ;
#4010 = CARTESIAN_POINT ( 'NONE',  ( -26.49328647146516147, 40.50686637268883317, -144.4416391455084181 ) ) ;
#4011 = ORIENTED_EDGE ( 'NONE', *, *, #18752, .F. ) ;
#4012 = CARTESIAN_POINT ( 'NONE',  ( -22.13782755527650892, 32.22299539119053691, -143.4425233068306227 ) ) ;
#4013 = EDGE_CURVE ( 'NONE', #22451, #14749, #15545, .T. ) ;
#4014 = ORIENTED_EDGE ( 'NONE', *, *, #8927, .T. ) ;
#4015 = CARTESIAN_POINT ( 'NONE',  ( -17.39900052719453072, -44.84364015992474606, -150.0552959529999555 ) ) ;
#4016 = ORIENTED_EDGE ( 'NONE', *, *, #2099, .T. ) ;
#4017 = SHAPE_DEFINITION_REPRESENTATION ( #16047, #15746 ) ;
#4018 = ORIENTED_EDGE ( 'NONE', *, *, #12890, .F. ) ;
#4019 = CARTESIAN_POINT ( 'NONE',  ( -29.68301555208973852, 36.92109708054170625, -140.1550845752986731 ) ) ;
#4020 = CARTESIAN_POINT ( 'NONE',  ( -31.00000000000000000, -36.00000000000000000, -149.5552959529999839 ) ) ;
#4021 = CARTESIAN_POINT ( 'NONE',  ( -20.60824191589999899, -4.000000000000000000, -146.2257682199999920 ) ) ;
#4022 = FACE_OUTER_BOUND ( 'NONE', #6398, .T. ) ;
#4023 = CARTESIAN_POINT ( 'NONE',  ( -2.499999999929999994, 31.50000000000000000, -138.0552959530000123 ) ) ;
#4024 = CARTESIAN_POINT ( 'NONE',  ( 7.750000000030000002, -37.98606797749999942, -137.0552959530000123 ) ) ;
#4025 = ORIENTED_EDGE ( 'NONE', *, *, #6716, .T. ) ;
#4026 = DIRECTION ( 'NONE',  ( 0.8571428571427679444, 0.5150787536378610421, -1.934960128632415569E-12 ) ) ;
#4027 = AXIS2_PLACEMENT_3D ( 'NONE', #22435, #8134, #6245 ) ;
#4028 = CARTESIAN_POINT ( 'NONE',  ( 22.68320006080000084, -24.50000000000000000, -148.5552959529999839 ) ) ;
#4029 = ORIENTED_EDGE ( 'NONE', *, *, #12431, .T. ) ;
#4030 = DIRECTION ( 'NONE',  ( 0.000000000000000000, 0.000000000000000000, 1.000000000000000000 ) ) ;
#4031 = CARTESIAN_POINT ( 'NONE',  ( -12.08222824379999949, 38.77433534089999512, -148.2726881729999775 ) ) ;
#4032 = EDGE_CURVE ( 'NONE', #1892, #15749, #20915, .T. ) ;
#4033 = DIRECTION ( 'NONE',  ( 2.507771768020000122E-12, 0.000000000000000000, -1.000000000000000000 ) ) ;
#4034 = DIRECTION ( 'NONE',  ( 8.955190032049260996E-12, -9.104778821548929412E-13, 1.000000000000000000 ) ) ;
#4035 = EDGE_LOOP ( 'NONE', ( #11037, #9057, #10491, #13868 ) ) ;
#4036 = CARTESIAN_POINT ( 'NONE',  ( -0.9999999999639999082, 20.50000000000000000, -136.0552959530000123 ) ) ;
#4037 = CARTESIAN_POINT ( 'NONE',  ( 8.750000000030000891, -44.75000000000000000, -136.0552959530000123 ) ) ;
#4038 = VERTEX_POINT ( 'NONE', #23046 ) ;
#4039 = DIRECTION ( 'NONE',  ( 1.000000000000000000, 0.000000000000000000, -4.510774274160000731E-12 ) ) ;
#4040 = CARTESIAN_POINT ( 'NONE',  ( -28.94327676059999988, 35.53474617860000251, -140.7339624629999832 ) ) ;
#4041 = PLANE ( 'NONE',  #6784 ) ;
#4042 = AXIS2_PLACEMENT_3D ( 'NONE', #17368, #13683, #2630 ) ;
#4043 = CARTESIAN_POINT ( 'NONE',  ( -21.19005019800000156, 41.30866696430000218, -143.6114845980000041 ) ) ;
#4044 = CIRCLE ( 'NONE', #10471, 1.500000000000001332 ) ;
#4045 = VERTEX_POINT ( 'NONE', #22811 ) ;
#4046 = CARTESIAN_POINT ( 'NONE',  ( -27.21970299319120912, 36.21690482628893193, -147.5085197383852176 ) ) ;
#4047 = CARTESIAN_POINT ( 'NONE',  ( 19.13369214859999801, 50.50000000000000000, -142.8052959529999839 ) ) ;
#4048 = ORIENTED_EDGE ( 'NONE', *, *, #12119, .F. ) ;
#4049 = FACE_OUTER_BOUND ( 'NONE', #14988, .T. ) ;
#4050 = DIRECTION ( 'NONE',  ( 2.507771768019999718E-12, 1.592654864209999947E-17, -1.000000000000000000 ) ) ;
#4051 = CARTESIAN_POINT ( 'NONE',  ( -5.246332635998737892, 43.48990303079973074, -136.0552959529881889 ) ) ;
#4052 = ORIENTED_EDGE ( 'NONE', *, *, #22890, .T. ) ;
#4053 = CARTESIAN_POINT ( 'NONE',  ( -31.50000000000000000, -36.00000000000000000, -137.0552959530000123 ) ) ;
#4054 = CARTESIAN_POINT ( 'NONE',  ( -4.021770264099999714, -29.17051924670000318, -142.5552959529999839 ) ) ;
#4055 = ORIENTED_EDGE ( 'NONE', *, *, #11777, .T. ) ;
#4056 = CIRCLE ( 'NONE', #7099, 0.7500000000000006661 ) ;
#4057 = ORIENTED_EDGE ( 'NONE', *, *, #3362, .F. ) ;
#4058 = CARTESIAN_POINT ( 'NONE',  ( -23.51619327739999932, 36.94101002280000046, -140.1031831869999849 ) ) ;
#4059 = EDGE_CURVE ( 'NONE', #4528, #20985, #9745, .T. ) ;
#4060 = PLANE ( 'NONE',  #13489 ) ;
#4061 = CARTESIAN_POINT ( 'NONE',  ( -7.500000000000000000, 42.50000000000000000, -150.0552959529999839 ) ) ;
#4062 = CARTESIAN_POINT ( 'NONE',  ( 7.436216203403632541, 35.94246666510559152, -141.7899860742952853 ) ) ;
#4063 = ORIENTED_EDGE ( 'NONE', *, *, #16184, .T. ) ;
#4064 = SURFACE_STYLE_FILL_AREA ( #20368 ) ;
#4065 = FACE_OUTER_BOUND ( 'NONE', #6237, .T. ) ;
#4066 = LINE ( 'NONE', #20489, #15883 ) ;
#4067 = CYLINDRICAL_SURFACE ( 'NONE', #1600, 7.500000000000005329 ) ;
#4068 = CARTESIAN_POINT ( 'NONE',  ( -24.07371653998410821, 40.87477276122073278, -141.8080750009974906 ) ) ;
#4069 = CARTESIAN_POINT ( 'NONE',  ( -16.13502618060000060, 32.80445174449999968, -146.2787800969999807 ) ) ;
#4070 = VECTOR ( 'NONE', #19576, 1000.000000000000000 ) ;
#4071 = PRESENTATION_LAYER_ASSIGNMENT (  '', '', ( #18141 ) ) ;
#4072 = DIRECTION ( 'NONE',  ( 0.000000000000000000, 1.000000000000000000, 0.000000000000000000 ) ) ;
#4073 = CARTESIAN_POINT ( 'NONE',  ( 4.750000000030000002, -2.273736754430000208E-12, -136.0552959530000123 ) ) ;
#4074 = CYLINDRICAL_SURFACE ( 'NONE', #923, 35.00000000000000000 ) ;
#4075 = ORIENTED_EDGE ( 'NONE', *, *, #23457, .F. ) ;
#4076 = CARTESIAN_POINT ( 'NONE',  ( -4.780317782130000914, 38.61135856239999953, -140.5115181619999873 ) ) ;
#4077 = DIRECTION ( 'NONE',  ( 1.000000000000000000, 0.000000000000000000, -1.522591576628786004E-13 ) ) ;
#4078 = VERTEX_POINT ( 'NONE', #20789 ) ;
#4079 = DIRECTION ( 'NONE',  ( 1.000000000000000000, 0.000000000000000000, 0.000000000000000000 ) ) ;
#4080 = CARTESIAN_POINT ( 'NONE',  ( -21.89685178202452320, 37.04474463553799524, -147.4979728336869869 ) ) ;
#4081 = CARTESIAN_POINT ( 'NONE',  ( -31.00000000000000000, 26.50000000000000000, -149.5552959529999839 ) ) ;
#4082 = ORIENTED_EDGE ( 'NONE', *, *, #20435, .T. ) ;
#4083 = CARTESIAN_POINT ( 'NONE',  ( -12.71428973609129365, 32.54945626905336553, -144.6365914293318440 ) ) ;
#4084 = AXIS2_PLACEMENT_3D ( 'NONE', #15245, #11765, #15358 ) ;
#4085 = ADVANCED_FACE ( 'NONE', ( #4606 ), #11845, .T. ) ;
#4086 = CARTESIAN_POINT ( 'NONE',  ( -2.500000000000000000, 40.00000000000000000, -151.0552959529999839 ) ) ;
#4087 = AXIS2_PLACEMENT_3D ( 'NONE', #2867, #15597, #19406 ) ;
#4088 = CARTESIAN_POINT ( 'NONE',  ( 13.13369214859999978, 51.50000000000000000, -137.0552959530000123 ) ) ;
#4089 = CARTESIAN_POINT ( 'NONE',  ( 4.374398326270000581, -26.09174856970000178, -144.5552959529999839 ) ) ;
#4090 = EDGE_CURVE ( 'NONE', #13352, #13032, #9939, .T. ) ;
#4091 = CARTESIAN_POINT ( 'NONE',  ( -13.86630785130000021, 51.00000000000000000, -137.0552959530000123 ) ) ;
#4092 = CARTESIAN_POINT ( 'NONE',  ( 20.31210873290000052, -31.32069079449999904, -147.0552959529999839 ) ) ;
#4093 = VERTEX_POINT ( 'NONE', #17446 ) ;
#4094 = CARTESIAN_POINT ( 'NONE',  ( -28.38533628227742867, 35.33089335701146894, -147.9595813284715007 ) ) ;
#4095 = ORIENTED_EDGE ( 'NONE', *, *, #21142, .T. ) ;
#4096 = ORIENTED_EDGE ( 'NONE', *, *, #20009, .F. ) ;
#4097 = CARTESIAN_POINT ( 'NONE',  ( -14.11967125418341951, 36.98834135281187940, -140.5455248811661875 ) ) ;
#4098 = PLANE ( 'NONE',  #16034 ) ;
#4099 = PLANE ( 'NONE',  #17649 ) ;
#4100 = VERTEX_POINT ( 'NONE', #11964 ) ;
#4101 = DIRECTION ( 'NONE',  ( 1.000000000000000000, 0.000000000000000000, -2.775557561562892298E-14 ) ) ;
#4102 = CARTESIAN_POINT ( 'NONE',  ( -7.816799939239999162, 0.9999999999989999111, -150.0552959529999839 ) ) ;
#4103 = VECTOR ( 'NONE', #102, 1000.000000000000000 ) ;
#4104 = VERTEX_POINT ( 'NONE', #8273 ) ;
#4105 = CARTESIAN_POINT ( 'NONE',  ( -20.71903412364733299, 37.77148386094349064, -140.0779489345810589 ) ) ;
#4106 = CARTESIAN_POINT ( 'NONE',  ( 9.356675081444274511, 38.23132590060392033, -141.8794674813294989 ) ) ;
#4107 = CARTESIAN_POINT ( 'NONE',  ( -18.85469010170000459, 37.03971195569999963, -148.4264296979999926 ) ) ;
#4108 = DIRECTION ( 'NONE',  ( -2.808280234689999718E-18, 1.000000000000000000, 1.592654863519999645E-17 ) ) ;
#4109 = ADVANCED_FACE ( 'NONE', ( #6618 ), #18878, .T. ) ;
#4110 = ORIENTED_EDGE ( 'NONE', *, *, #6634, .T. ) ;
#4111 = CIRCLE ( 'NONE', #15900, 0.5000000000000004441 ) ;
#4112 = LINE ( 'NONE', #14835, #9155 ) ;
#4113 = BREP_WITH_VOIDS ( 'NONE', #20590, ( #8159, #13114 ) );
#4114 = STYLED_ITEM ( 'NONE', ( #5784 ), #20181 ) ;
#4115 = VERTEX_POINT ( 'NONE', #15319 ) ;
#4116 = CARTESIAN_POINT ( 'NONE',  ( 8.750000000000001776, -47.26504245777761071, -150.0552959530000123 ) ) ;
#4117 = ORIENTED_EDGE ( 'NONE', *, *, #984, .F. ) ;
#4118 = CARTESIAN_POINT ( 'NONE',  ( -26.67031178456957008, 38.52782902798677611, -147.6692609235824989 ) ) ;
#4119 = ORIENTED_EDGE ( 'NONE', *, *, #7673, .F. ) ;
#4120 = CYLINDRICAL_SURFACE ( 'NONE', #9822, 5.999999999999999112 ) ;
#4121 = EDGE_CURVE ( 'NONE', #13431, #13154, #4479, .T. ) ;
#4122 = EDGE_LOOP ( 'NONE', ( #20523, #16555, #6073, #5554 ) ) ;
#4123 = PLANE ( 'NONE',  #6839 ) ;
#4124 = ORIENTED_EDGE ( 'NONE', *, *, #16868, .T. ) ;
#4125 = APPLICATION_PROTOCOL_DEFINITION ( 'draft international standard', 'automotive_design', 1998, #18008 ) ;
#4126 = ORIENTED_EDGE ( 'NONE', *, *, #2070, .T. ) ;
#4127 = DIRECTION ( 'NONE',  ( 1.000000000000000000, 0.000000000000000000, 0.000000000000000000 ) ) ;
#4128 = CARTESIAN_POINT ( 'NONE',  ( -5.070907855439999778, -22.41528233759999722, -148.5552959529999839 ) ) ;
#4129 = LINE ( 'NONE', #20437, #11090 ) ;
#4130 = LINE ( 'NONE', #7693, #12856 ) ;
#4131 = CARTESIAN_POINT ( 'NONE',  ( -7.138130562210037944, 35.21651592843031864, -148.3216512489436241 ) ) ;
#4132 = VECTOR ( 'NONE', #7924, 1000.000000000000000 ) ;
#4133 = EDGE_CURVE ( 'NONE', #17961, #7102, #8402, .T. ) ;
#4134 = CARTESIAN_POINT ( 'NONE',  ( -7.671834446767463511, 37.96637496773506371, -139.6710333262370796 ) ) ;
#4135 = VERTEX_POINT ( 'NONE', #23397 ) ;
#4136 = ADVANCED_FACE ( 'NONE', ( #3289 ), #8621, .T. ) ;
#4137 = VECTOR ( 'NONE', #14049, 1000.000000000000000 ) ;
#4138 = CYLINDRICAL_SURFACE ( 'NONE', #17052, 2.499999999999999112 ) ;
#4139 = AXIS2_PLACEMENT_3D ( 'NONE', #2505, #20585, #20354 ) ;
#4140 = ADVANCED_FACE ( 'NONE', ( #1755 ), #8744, .F. ) ;
#4141 = PLANE ( 'NONE',  #19347 ) ;
#4142 = AXIS2_PLACEMENT_3D ( 'NONE', #16291, #12466, #8775 ) ;
#4143 = EDGE_CURVE ( 'NONE', #10222, #3729, #18044, .T. ) ;
#4144 = CARTESIAN_POINT ( 'NONE',  ( 3.038243779794036037, -3.109320143290841276, -136.0552959530068620 ) ) ;
#4145 = ORIENTED_EDGE ( 'NONE', *, *, #10917, .T. ) ;
#4146 = CARTESIAN_POINT ( 'NONE',  ( -11.09667937100654989, 38.99134170279717182, -139.7423566497915886 ) ) ;
#4147 = CARTESIAN_POINT ( 'NONE',  ( -17.59229711595959955, 39.34301127023525879, -147.3183469250201654 ) ) ;
#4148 = CARTESIAN_POINT ( 'NONE',  ( -29.26198848999914759, 40.69426223529025322, -144.9540979635152098 ) ) ;
#4149 = ORIENTED_EDGE ( 'NONE', *, *, #1588, .T. ) ;
#4150 = DIRECTION ( 'NONE',  ( -0.07970438983373200059, -0.9968185442904001770, 8.268372250843320857E-13 ) ) ;
#4151 = LINE ( 'NONE', #14870, #10079 ) ;
#4152 = VECTOR ( 'NONE', #12381, 1000.000000000000000 ) ;
#4153 = ORIENTED_EDGE ( 'NONE', *, *, #12358, .F. ) ;
#4154 = LINE ( 'NONE', #2386, #15576 ) ;
#4155 = DIRECTION ( 'NONE',  ( 1.000000000000000000, 0.000000000000000000, -8.955799065309598247E-12 ) ) ;
#4156 = ORIENTED_EDGE ( 'NONE', *, *, #7538, .T. ) ;
#4157 = LINE ( 'NONE', #22015, #4888 ) ;
#4158 = EDGE_CURVE ( 'NONE', #21164, #3905, #23516, .T. ) ;
#4159 = VECTOR ( 'NONE', #13233, 1000.000000000000000 ) ;
#4160 = CARTESIAN_POINT ( 'NONE',  ( -20.45144833149999997, 36.94873838139999833, -139.8044047869999815 ) ) ;
#4161 = ORIENTED_EDGE ( 'NONE', *, *, #506, .T. ) ;
#4162 = EDGE_CURVE ( 'NONE', #6084, #13875, #23160, .T. ) ;
#4163 = VECTOR ( 'NONE', #17355, 1000.000000000000227 ) ;
#4164 = LINE ( 'NONE', #4047, #20930 ) ;
#4165 = ORIENTED_EDGE ( 'NONE', *, *, #2391, .F. ) ;
#4166 = AXIS2_PLACEMENT_3D ( 'NONE', #16030, #1530, #4845 ) ;
#4167 = DIRECTION ( 'NONE',  ( -2.257144641399999941E-12, 8.049635416090000264E-35, -1.000000000000000000 ) ) ;
#4168 = DIRECTION ( 'NONE',  ( -1.000000000000000000, 0.000000000000000000, 0.000000000000000000 ) ) ;
#4169 = DIRECTION ( 'NONE',  ( 0.4144957952930628520, -0.9100512269561374934, 6.800116025829078761E-13 ) ) ;
#4170 = VERTEX_POINT ( 'NONE', #5185 ) ;
#4171 = ADVANCED_FACE ( 'NONE', ( #4962 ), #21503, .F. ) ;
#4172 = CARTESIAN_POINT ( 'NONE',  ( 12.50000000010000001, 16.89444872450000190, -143.5552959529999839 ) ) ;
#4173 = EDGE_CURVE ( 'NONE', #14517, #5601, #12435, .T. ) ;
#4174 = CARTESIAN_POINT ( 'NONE',  ( -32.50000000000000000, 10.25000000000000000, -137.0552959530000123 ) ) ;
#4175 = ORIENTED_EDGE ( 'NONE', *, *, #21775, .F. ) ;
#4176 = VECTOR ( 'NONE', #21751, 1000.000000000000000 ) ;
#4177 = EDGE_CURVE ( 'NONE', #15326, #8394, #19709, .T. ) ;
#4178 = EDGE_LOOP ( 'NONE', ( #11998, #7794, #7453, #797 ) ) ;
#4179 = AXIS2_PLACEMENT_3D ( 'NONE', #7301, #12761, #7176 ) ;
#4180 = AXIS2_PLACEMENT_3D ( 'NONE', #19676, #3373, #3257 ) ;
#4181 = CARTESIAN_POINT ( 'NONE',  ( -23.01895658101113540, 35.59613479725317120, -140.8867697970091797 ) ) ;
#4182 = DIRECTION ( 'NONE',  ( 0.000000000000000000, 0.000000000000000000, 1.000000000000000000 ) ) ;
#4183 = VECTOR ( 'NONE', #21903, 1000.000000000000000 ) ;
#4184 = VECTOR ( 'NONE', #6760, 1000.000000000000000 ) ;
#4185 = DIRECTION ( 'NONE',  ( -1.000000000000000000, 0.000000000000000000, 0.000000000000000000 ) ) ;
#4186 = DIRECTION ( 'NONE',  ( 0.000000000000000000, 1.000000000000000000, 0.000000000000000000 ) ) ;
#4187 = VERTEX_POINT ( 'NONE', #14122 ) ;
#4188 = FACE_OUTER_BOUND ( 'NONE', #11119, .T. ) ;
#4189 = DIRECTION ( 'NONE',  ( -2.842170943040000002E-14, -3.570477247189999985E-13, -1.000000000000000000 ) ) ;
#4190 = DIRECTION ( 'NONE',  ( 0.000000000000000000, -1.000000000000000000, 0.000000000000000000 ) ) ;
#4191 = CARTESIAN_POINT ( 'NONE',  ( 12.88080765325204879, 38.01462304342913967, -136.0552959530290593 ) ) ;
#4192 = CARTESIAN_POINT ( 'NONE',  ( -23.85957119133389881, 39.58299060703604511, -140.4713739358294333 ) ) ;
#4193 = CARTESIAN_POINT ( 'NONE',  ( -15.46352699119206697, 34.98433354313474553, -148.3064882238327016 ) ) ;
#4194 = CARTESIAN_POINT ( 'NONE',  ( -17.03115501030000090, 35.19590004879999867, -139.8299307730000010 ) ) ;
#4195 = FACE_OUTER_BOUND ( 'NONE', #22129, .T. ) ;
#4196 = CARTESIAN_POINT ( 'NONE',  ( -7.499999999969999109, 42.50000000000000000, -136.5552959530000123 ) ) ;
#4197 = CARTESIAN_POINT ( 'NONE',  ( 1.354168148130000082, -20.95195702430000040, -144.0552959529999839 ) ) ;
#4198 = VECTOR ( 'NONE', #18442, 1000.000000000000114 ) ;
#4199 = AXIS2_PLACEMENT_3D ( 'NONE', #21594, #10738, #18018 ) ;
#4200 = VERTEX_POINT ( 'NONE', #12554 ) ;
#4201 = EDGE_CURVE ( 'NONE', #18280, #4867, #15996, .T. ) ;
#4202 = CARTESIAN_POINT ( 'NONE',  ( -5.801925844418948763, 39.15421101755954680, -147.0556221922513487 ) ) ;
#4203 = CARTESIAN_POINT ( 'NONE',  ( 7.085709294149999060, -13.66851965709999916, -143.5552959529999839 ) ) ;
#4204 = EDGE_CURVE ( 'NONE', #19876, #3906, #1581, .T. ) ;
#4205 = ORIENTED_EDGE ( 'NONE', *, *, #15447, .F. ) ;
#4206 = LINE ( 'NONE', #2433, #17133 ) ;
#4207 = CARTESIAN_POINT ( 'NONE',  ( -22.10875017890000294, 36.18377167419999552, -148.1739623899999856 ) ) ;
#4208 = DIRECTION ( 'NONE',  ( 0.9944529286486341046, -0.1051825684329612265, -4.469111776238355154E-12 ) ) ;
#4209 = ORIENTED_EDGE ( 'NONE', *, *, #18818, .T. ) ;
#4210 = DIRECTION ( 'NONE',  ( -1.000000000000000000, 5.094701932209999624E-24, 2.257144641399999941E-12 ) ) ;
#4211 = CARTESIAN_POINT ( 'NONE',  ( 12.49993271304849252, 36.89748944252419705, -150.0552959529999839 ) ) ;
#4212 = CARTESIAN_POINT ( 'NONE',  ( -9.282104535849999394, -16.71402168319999859, -144.5552959529999839 ) ) ;
#4213 = CARTESIAN_POINT ( 'NONE',  ( -4.499999999959999109, 34.00000000000000000, -151.5552959529999839 ) ) ;
#4214 = VECTOR ( 'NONE', #2079, 1000.000000000000000 ) ;
#4215 = CARTESIAN_POINT ( 'NONE',  ( -18.35824191589999899, -34.50000000000000000, -146.3157682190000060 ) ) ;
#4216 = ORIENTED_EDGE ( 'NONE', *, *, #18880, .T. ) ;
#4217 = CARTESIAN_POINT ( 'NONE',  ( -27.77832206610000298, 37.03059619289999915, -147.6270870419999710 ) ) ;
#4218 = PRODUCT ( 'Slotted Screw', 'Slotted Screw', '', ( #22218 ) ) ;
#4219 = ADVANCED_FACE ( 'NONE', ( #7093 ), #9096, .F. ) ;
#4220 = ORIENTED_EDGE ( 'NONE', *, *, #12349, .T. ) ;
#4221 = CARTESIAN_POINT ( 'NONE',  ( -14.26108793495632554, 34.19565738791286691, -140.4808705499285111 ) ) ;
#4222 = PLANE ( 'NONE',  #16412 ) ;
#4223 = CARTESIAN_POINT ( 'NONE',  ( -30.49999999990000177, 47.50000000000000000, -147.5552959529999839 ) ) ;
#4224 = EDGE_CURVE ( 'NONE', #14338, #2164, #14719, .T. ) ;
#4225 = ORIENTED_EDGE ( 'NONE', *, *, #11237, .F. ) ;
#4226 = EDGE_CURVE ( 'NONE', #15863, #2602, #17801, .T. ) ;
#4227 = CARTESIAN_POINT ( 'NONE',  ( 25.11896946145980891, 38.01480899506201183, -136.0552959530567421 ) ) ;
#4228 = CARTESIAN_POINT ( 'NONE',  ( 18.95053822279999878, -51.50000000000000000, -149.8052959529999839 ) ) ;
#4229 = EDGE_CURVE ( 'NONE', #21917, #14118, #5306, .T. ) ;
#4230 = ORIENTED_EDGE ( 'NONE', *, *, #15873, .T. ) ;
#4231 = CIRCLE ( 'NONE', #23239, 8.176568160359998672 ) ;
#4232 = CARTESIAN_POINT ( 'NONE',  ( -20.08037650815199981, 40.50744741039175523, -142.1449807696052119 ) ) ;
#4233 = CARTESIAN_POINT ( 'NONE',  ( 9.116160410115874413, 38.36768097678178435, -141.9625758178371484 ) ) ;
#4234 = FACE_BOUND ( 'NONE', #6141, .T. ) ;
#4235 = CARTESIAN_POINT ( 'NONE',  ( 4.999999999879999990, -1.500000000000000000, -135.0552959530000123 ) ) ;
#4236 = CARTESIAN_POINT ( 'NONE',  ( -31.00000000000000000, -7.105427357599999217E-15, -149.5552959529999839 ) ) ;
#4237 = ORIENTED_EDGE ( 'NONE', *, *, #8774, .T. ) ;
#4238 = FACE_OUTER_BOUND ( 'NONE', #1795, .T. ) ;
#4239 = ORIENTED_EDGE ( 'NONE', *, *, #12303, .F. ) ;
#4240 = LINE ( 'NONE', #914, #12844 ) ;
#4241 = AXIS2_PLACEMENT_3D ( 'NONE', #15009, #22389, #2067 ) ;
#4242 = VECTOR ( 'NONE', #22137, 1000.000000000000000 ) ;
#4243 = ORIENTED_EDGE ( 'NONE', *, *, #17001, .F. ) ;
#4244 =( NAMED_UNIT ( * ) PLANE_ANGLE_UNIT ( ) SI_UNIT ( $, .RADIAN. ) );
#4245 = ORIENTED_EDGE ( 'NONE', *, *, #1560, .T. ) ;
#4246 = CARTESIAN_POINT ( 'NONE',  ( -22.70111404018277668, 32.50422370117523485, -144.5121409266673140 ) ) ;
#4247 = ORIENTED_EDGE ( 'NONE', *, *, #14914, .T. ) ;
#4248 = DIRECTION ( 'NONE',  ( 0.000000000000000000, 2.256988247090000272E-12, 1.000000000000000000 ) ) ;
#4249 = ORIENTED_EDGE ( 'NONE', *, *, #15459, .T. ) ;
#4250 = ORIENTED_EDGE ( 'NONE', *, *, #9936, .F. ) ;
#4251 = CARTESIAN_POINT ( 'NONE',  ( -27.60583033794648600, 37.01000650950496862, -148.6900182104589589 ) ) ;
#4252 = CARTESIAN_POINT ( 'NONE',  ( -13.86630785130000021, -50.50000000000000000, -136.5552959530000123 ) ) ;
#4253 = CARTESIAN_POINT ( 'NONE',  ( 11.45511797032570911, 26.15112731433314153, -150.0552959529999839 ) ) ;
#4254 = ADVANCED_FACE ( 'NONE', ( #12208 ), #1395, .T. ) ;
#4255 = DIRECTION ( 'NONE',  ( -8.955190032050000935E-12, 9.104778821549999739E-13, -1.000000000000000000 ) ) ;
#4256 = CARTESIAN_POINT ( 'NONE',  ( -7.243544775885156994, 34.37889476601232275, -147.8566374764138516 ) ) ;
#4257 = CARTESIAN_POINT ( 'NONE',  ( 19.27350934360000068, 50.38169314270000143, -149.5552959529999839 ) ) ;
#4258 = ORIENTED_EDGE ( 'NONE', *, *, #13581, .T. ) ;
#4259 = CARTESIAN_POINT ( 'NONE',  ( 6.500000000140000012, 12.50000000000000000, -146.5552959529999839 ) ) ;
#4260 = VECTOR ( 'NONE', #2468, 1000.000000000000000 ) ;
#4261 = CIRCLE ( 'NONE', #11460, 6.000000000000001776 ) ;
#4262 = AXIS2_PLACEMENT_3D ( 'NONE', #22394, #11194, #22162 ) ;
#4263 = PRODUCT_RELATED_PRODUCT_CATEGORY ( 'part', '', ( #18224 ) ) ;
#4264 = DIRECTION ( 'NONE',  ( 1.000000000000000000, 0.000000000000000000, -2.257157423930000049E-12 ) ) ;
#4265 = EDGE_CURVE ( 'NONE', #12804, #15239, #1521, .T. ) ;
#4266 = DIRECTION ( 'NONE',  ( -0.9954742291034677226, 0.09503188512734457583, 4.502513436702118395E-12 ) ) ;
#4267 = VERTEX_POINT ( 'NONE', #4546 ) ;
#4268 = CARTESIAN_POINT ( 'NONE',  ( -12.74435279828027490, 38.88449211440367748, -148.3283390160977717 ) ) ;
#4269 = CARTESIAN_POINT ( 'NONE',  ( 31.50000000000000000, -0.03620104880649999829, -136.0552959530000123 ) ) ;
#4270 = CARTESIAN_POINT ( 'NONE',  ( -34.50000000000000000, 14.95885107719999851, -142.3001308290000111 ) ) ;
#4271 = EDGE_LOOP ( 'NONE', ( #12112, #13477, #16670, #13883 ) ) ;
#4272 = DIRECTION ( 'NONE',  ( 1.000000000000000000, 0.000000000000000000, -2.257453483404485639E-12 ) ) ;
#4273 = PLANE ( 'NONE',  #14283 ) ;
#4274 = EDGE_CURVE ( 'NONE', #15302, #18787, #11703, .T. ) ;
#4275 = ORIENTED_EDGE ( 'NONE', *, *, #9679, .F. ) ;
#4276 = CARTESIAN_POINT ( 'NONE',  ( -21.50145757625659826, 36.99754792878884757, -147.3684231710527399 ) ) ;
#4277 = CARTESIAN_POINT ( 'NONE',  ( 16.64676602990000021, -18.64223989710000140, -144.0552959529999839 ) ) ;
#4278 = ORIENTED_EDGE ( 'NONE', *, *, #9231, .F. ) ;
#4279 = CARTESIAN_POINT ( 'NONE',  ( 4.468795199060000556, -26.40504320680000205, -143.5552959529999839 ) ) ;
#4280 = CARTESIAN_POINT ( 'NONE',  ( -21.90852802850000103, 37.90475843469999973, -148.1502781210000137 ) ) ;
#4281 = ORIENTED_EDGE ( 'NONE', *, *, #8768, .F. ) ;
#4282 = APPLICATION_PROTOCOL_DEFINITION ( 'draft international standard', 'automotive_design', 1998, #1438 ) ;
#4283 = AXIS2_PLACEMENT_3D ( 'NONE', #1426, #21528, #8771 ) ;
#4284 = DIRECTION ( 'NONE',  ( 1.000000000000000000, 0.000000000000000000, 0.000000000000000000 ) ) ;
#4285 = CARTESIAN_POINT ( 'NONE',  ( 19.13369214859999801, 51.50000000000000000, -136.0552959530000123 ) ) ;
#4286 = VERTEX_POINT ( 'NONE', #4426 ) ;
#4287 = DIRECTION ( 'NONE',  ( 0.000000000000000000, -1.000000000000000000, 0.000000000000000000 ) ) ;
#4288 = LINE ( 'NONE', #251, #3519 ) ;
#4289 = ADVANCED_FACE ( 'NONE', ( #17157 ), #21858, .T. ) ;
#4290 = CARTESIAN_POINT ( 'NONE',  ( -35.47299999999999898, 11.04196010839999964, -144.5552959529999839 ) ) ;
#4291 = ORIENTED_EDGE ( 'NONE', *, *, #17001, .T. ) ;
#4292 = CARTESIAN_POINT ( 'NONE',  ( -35.07300000000000040, 16.55147016440000129, -143.5552959529999839 ) ) ;
#4293 = CARTESIAN_POINT ( 'NONE',  ( 23.78818517497831664, -17.51387386319286321, -144.7152959530024816 ) ) ;
#4294 = ORIENTED_EDGE ( 'NONE', *, *, #13716, .T. ) ;
#4295 = EDGE_CURVE ( 'NONE', #19783, #6756, #4111, .T. ) ;
#4296 = STYLED_ITEM ( 'NONE', ( #10840 ), #3845 ) ;
#4297 = EDGE_LOOP ( 'NONE', ( #19857, #13519, #13271, #15796 ) ) ;
#4298 = FACE_OUTER_BOUND ( 'NONE', #17298, .T. ) ;
#4299 = FACE_OUTER_BOUND ( 'NONE', #1835, .T. ) ;
#4300 = FACE_OUTER_BOUND ( 'NONE', #5072, .T. ) ;
#4301 = FACE_OUTER_BOUND ( 'NONE', #5759, .T. ) ;
#4302 = ORIENTED_EDGE ( 'NONE', *, *, #18394, .F. ) ;
#4303 = CARTESIAN_POINT ( 'NONE',  ( -8.764836022000000781, 39.53398178709999655, -147.5842891229999907 ) ) ;
#4304 = EDGE_CURVE ( 'NONE', #12120, #8637, #2101, .T. ) ;
#4305 = DIRECTION ( 'NONE',  ( -0.9874789572432817186, 0.1577507813030449846, 2.191150709840624368E-14 ) ) ;
#4306 = DIRECTION ( 'NONE',  ( 1.000000000000000000, 0.000000000000000000, -2.257144641399999941E-12 ) ) ;
#4307 = CARTESIAN_POINT ( 'NONE',  ( -24.78261485200000180, 38.62237172060000034, -147.6366313890000015 ) ) ;
#4308 = ADVANCED_FACE ( 'NONE', ( #13578 ), #13031, .T. ) ;
#4309 = CARTESIAN_POINT ( 'NONE',  ( -15.25588521237791539, 34.19578262203260977, -147.5708427275093015 ) ) ;
#4310 = ADVANCED_FACE ( 'NONE', ( #11003 ), #9216, .F. ) ;
#4311 = CARTESIAN_POINT ( 'NONE',  ( -16.58211931832967068, 33.51686747480896855, -143.5423247306498240 ) ) ;
#4312 = ADVANCED_FACE ( 'NONE', ( #7668 ), #16594, .F. ) ;
#4313 = CARTESIAN_POINT ( 'NONE',  ( -20.23971019809999916, 35.09018026569999904, -140.0771129649999978 ) ) ;
#4314 = DIRECTION ( 'NONE',  ( 0.000000000000000000, 0.000000000000000000, 1.000000000000000000 ) ) ;
#4315 = VECTOR ( 'NONE', #19648, 1000.000000000000227 ) ;
#4316 = DIRECTION ( 'NONE',  ( 0.000000000000000000, 1.000000000000000000, 0.000000000000000000 ) ) ;
#4317 = VERTEX_POINT ( 'NONE', #86 ) ;
#4318 = CARTESIAN_POINT ( 'NONE',  ( -9.971101149771200767, 37.05360750094124000, -147.8421425034415790 ) ) ;
#4319 = CARTESIAN_POINT ( 'NONE',  ( -15.00000000000000000, -43.00000000000000000, -137.0552959530000123 ) ) ;
#4320 = ORIENTED_EDGE ( 'NONE', *, *, #8018, .T. ) ;
#4321 = CARTESIAN_POINT ( 'NONE',  ( 0.000000000000000000, -50.00000000000000000, -150.0552959529999839 ) ) ;
#4322 = CARTESIAN_POINT ( 'NONE',  ( -21.22299042056730300, 36.20661401050380590, -147.5479327630602029 ) ) ;
#4323 = PLANE ( 'NONE',  #9074 ) ;
#4324 = ORIENTED_EDGE ( 'NONE', *, *, #19785, .T. ) ;
#4325 = CARTESIAN_POINT ( 'NONE',  ( -12.79720822650000045, 32.99715178900000012, -146.4964997610000239 ) ) ;
#4326 = CARTESIAN_POINT ( 'NONE',  ( 13.13369214870000157, 50.50000000000000000, -136.5552959530000123 ) ) ;
#4327 = CARTESIAN_POINT ( 'NONE',  ( 0.1832000607640000001, 0.4999999999990000776, -149.3052959529999839 ) ) ;
#4328 = CARTESIAN_POINT ( 'NONE',  ( 32.50000000000000000, 0.000000000000000000, -136.0552959530000123 ) ) ;
#4329 = CARTESIAN_POINT ( 'NONE',  ( -6.072796602490000417, -14.62912504250000012, -144.0552959529999839 ) ) ;
#4330 = CARTESIAN_POINT ( 'NONE',  ( 9.763108217333922312, -36.11272049728156475, -150.0552959529999839 ) ) ;
#4331 = VECTOR ( 'NONE', #17475, 1000.000000000000000 ) ;
#4332 = VERTEX_POINT ( 'NONE', #18940 ) ;
#4333 = EDGE_CURVE ( 'NONE', #15560, #8780, #11225, .T. ) ;
#4334 = CARTESIAN_POINT ( 'NONE',  ( -27.70749540540193578, 36.02653024062528431, -148.6920955691318795 ) ) ;
#4335 = ORIENTED_EDGE ( 'NONE', *, *, #9812, .T. ) ;
#4336 = CARTESIAN_POINT ( 'NONE',  ( -13.67845320973112244, 33.33591541118190094, -146.4032996680919041 ) ) ;
#4337 = CARTESIAN_POINT ( 'NONE',  ( -22.10824191589186327, -4.000000000000000000, -149.4708568729739966 ) ) ;
#4338 = CARTESIAN_POINT ( 'NONE',  ( 22.00000000000000000, -20.50000000000000000, -137.0552959530000123 ) ) ;
#4339 = ORIENTED_EDGE ( 'NONE', *, *, #2443, .T. ) ;
#4340 = PLANE ( 'NONE',  #11011 ) ;
#4341 = DIRECTION ( 'NONE',  ( 0.000000000000000000, 0.8775825618903703162, 0.4794255386042076128 ) ) ;
#4342 = ORIENTED_EDGE ( 'NONE', *, *, #3446, .T. ) ;
#4343 = CARTESIAN_POINT ( 'NONE',  ( -20.65692115970000131, 38.75897267589999728, -140.0270467099999792 ) ) ;
#4344 = AXIS2_PLACEMENT_3D ( 'NONE', #8006, #15290, #6820 ) ;
#4345 = CARTESIAN_POINT ( 'NONE',  ( -17.75002847806602091, 38.41025389510169674, -140.6489478483555331 ) ) ;
#4346 = CARTESIAN_POINT ( 'NONE',  ( 0.000000000000000000, 42.50000000000000000, -150.0552959529999839 ) ) ;
#4347 =( BOUNDED_CURVE ( )  B_SPLINE_CURVE ( 5, ( #509, #7975, #389, #5960, #2418, #16908 ),
 .UNSPECIFIED., .F., .F. ) 
 B_SPLINE_CURVE_WITH_KNOTS ( ( 6, 6 ),
 ( 0.000000000000000000, 1.570796326521524344 ),
 .UNSPECIFIED. ) 
 CURVE ( )  GEOMETRIC_REPRESENTATION_ITEM ( )  RATIONAL_B_SPLINE_CURVE ( ( 1.000000000000000000, 0.6000000000696400493, 0.4000000000696400382, 0.3000000000522300425, 0.2500000000348200357, 0.2500000000000000000 ) ) 
 REPRESENTATION_ITEM ( '' )  );
#4348 = CARTESIAN_POINT ( 'NONE',  ( -32.50000000000000000, 1.000000000000000000, -143.3052959529999839 ) ) ;
#4349 = CARTESIAN_POINT ( 'NONE',  ( -25.51633159842389986, 34.96116192632524644, -141.2416905447548459 ) ) ;
#4350 = VERTEX_POINT ( 'NONE', #19063 ) ;
#4351 = EDGE_CURVE ( 'NONE', #473, #9406, #20731, .T. ) ;
#4352 = CARTESIAN_POINT ( 'NONE',  ( 1.133692148550000001, -50.50000000000000000, -136.0552959530000123 ) ) ;
#4353 = ORIENTED_EDGE ( 'NONE', *, *, #11404, .F. ) ;
#4354 = LINE ( 'NONE', #11706, #1848 ) ;
#4355 = VERTEX_POINT ( 'NONE', #20063 ) ;
#4356 = VERTEX_POINT ( 'NONE', #3760 ) ;
#4357 = CARTESIAN_POINT ( 'NONE',  ( -4.959431410700000598, -23.66636161550000139, -146.5552959529999839 ) ) ;
#4358 = ORIENTED_EDGE ( 'NONE', *, *, #19128, .T. ) ;
#4359 = CARTESIAN_POINT ( 'NONE',  ( -25.86630785139999844, -50.50000000000000000, -136.0552959530000123 ) ) ;
#4360 = VERTEX_POINT ( 'NONE', #2774 ) ;
#4361 = ORIENTED_EDGE ( 'NONE', *, *, #9154, .F. ) ;
#4362 = CARTESIAN_POINT ( 'NONE',  ( -27.97930636479113531, 38.80653505726444763, -147.9089998809065776 ) ) ;
#4363 = DIRECTION ( 'NONE',  ( 2.257749542879999954E-12, 0.000000000000000000, 1.000000000000000000 ) ) ;
#4364 = DIRECTION ( 'NONE',  ( 1.000000000000000000, 0.000000000000000000, -2.257453483404482811E-12 ) ) ;
#4365 = DIRECTION ( 'NONE',  ( -1.000000000000000000, 0.000000000000000000, 0.000000000000000000 ) ) ;
#4366 = CARTESIAN_POINT ( 'NONE',  ( -7.462508610423953748, 33.01377392928537802, -146.5273241004201168 ) ) ;
#4367 = CARTESIAN_POINT ( 'NONE',  ( -7.856058713499369794, 37.01980778200731237, -139.4032252962407483 ) ) ;
#4368 = ORIENTED_EDGE ( 'NONE', *, *, #22047, .T. ) ;
#4369 = CARTESIAN_POINT ( 'NONE',  ( -1.753667363961266989, 45.51009696919363989, -150.0552959529999839 ) ) ;
#4370 = CARTESIAN_POINT ( 'NONE',  ( 32.50000000000000000, -21.03620104879999886, -137.0552959530000123 ) ) ;
#4371 = LINE ( 'NONE', #9035, #23538 ) ;
#4372 = ORIENTED_EDGE ( 'NONE', *, *, #9872, .F. ) ;
#4373 = B_SPLINE_CURVE_WITH_KNOTS ( 'NONE', 3,
 ( #5165, #12414, #14334, #17911 ),
 .UNSPECIFIED., .F., .F.,
 ( 4, 4 ),
 ( 0.000000000000000000, 0.8059436278830001132 ),
 .UNSPECIFIED. ) ;
#4374 = EDGE_CURVE ( 'NONE', #10468, #3556, #18284, .T. ) ;
#4375 = CARTESIAN_POINT ( 'NONE',  ( -17.89449577229860111, 36.92509720026602338, -147.9522036891450227 ) ) ;
#4376 = CARTESIAN_POINT ( 'NONE',  ( -2.499999999929999994, 32.75000000000000000, -138.0552959530000123 ) ) ;
#4377 = ORIENTED_EDGE ( 'NONE', *, *, #6622, .T. ) ;
#4378 = PRESENTATION_STYLE_ASSIGNMENT (( #7936 ) ) ;
#4379 = EDGE_CURVE ( 'NONE', #5378, #22981, #14383, .T. ) ;
#4380 = LINE ( 'NONE', #22238, #2153 ) ;
#4381 = ORIENTED_EDGE ( 'NONE', *, *, #23081, .F. ) ;
#4382 = DIRECTION ( 'NONE',  ( 0.000000000000000000, 1.000000000000000000, 0.000000000000000000 ) ) ;
#4383 = CARTESIAN_POINT ( 'NONE',  ( 20.57808196999505412, -21.28524365307785260, -150.0552959530000123 ) ) ;
#4384 = ORIENTED_EDGE ( 'NONE', *, *, #18993, .F. ) ;
#4385 = DIRECTION ( 'NONE',  ( 0.000000000000000000, -1.000000000000000000, 8.159623473500000156E-13 ) ) ;
#4386 = CARTESIAN_POINT ( 'NONE',  ( -19.70010857004652394, 39.59599344006944222, -140.6831085099040308 ) ) ;
#4387 = EDGE_LOOP ( 'NONE', ( #11899, #9813, #15038, #4737, #7332 ) ) ;
#4388 = CARTESIAN_POINT ( 'NONE',  ( -28.80902675602211715, 36.08666534565443840, -139.5659208845989951 ) ) ;
#4389 = FACE_OUTER_BOUND ( 'NONE', #5302, .T. ) ;
#4390 = ORIENTED_EDGE ( 'NONE', *, *, #229, .F. ) ;
#4391 = CARTESIAN_POINT ( 'NONE',  ( -33.50000000000000000, 26.00000000000000000, -141.5552959529999839 ) ) ;
#4392 = VECTOR ( 'NONE', #9744, 999.9999999999998863 ) ;
#4393 = CARTESIAN_POINT ( 'NONE',  ( -17.01442029460000072, -1.500000000000000000, -147.5657682190000060 ) ) ;
#4394 = ORIENTED_EDGE ( 'NONE', *, *, #11852, .F. ) ;
#4395 = CIRCLE ( 'NONE', #21512, 2.000000000000001776 ) ;
#4396 = DIRECTION ( 'NONE',  ( -1.000000000000000000, 0.000000000000000000, -2.245315044929999938E-12 ) ) ;
#4397 = ORIENTED_EDGE ( 'NONE', *, *, #109, .F. ) ;
#4398 = DIRECTION ( 'NONE',  ( -1.211690350419999855E-27, -2.765629237169980113E-27, 1.000000000000000000 ) ) ;
#4399 = EDGE_LOOP ( 'NONE', ( #7208, #944, #20037, #2985 ) ) ;
#4400 = EDGE_CURVE ( 'NONE', #13712, #16611, #7435, .T. ) ;
#4401 = VERTEX_POINT ( 'NONE', #18390 ) ;
#4402 = CARTESIAN_POINT ( 'NONE',  ( 1.878640834937223669, -1.989143058887305804, -150.0552959529999839 ) ) ;
#4403 = CARTESIAN_POINT ( 'NONE',  ( -34.50000000000000000, -63.54114892279999793, -142.3001308290000111 ) ) ;
#4404 = CARTESIAN_POINT ( 'NONE',  ( -13.59981317924081701, 37.05039483956773694, -139.6306434366684357 ) ) ;
#4405 = DIRECTION ( 'NONE',  ( -1.000000000000000000, 0.000000000000000000, -2.245315044999999693E-12 ) ) ;
#4406 = VECTOR ( 'NONE', #12477, 1000.000000000000000 ) ;
#4407 = EDGE_LOOP ( 'NONE', ( #20782, #9100, #14886, #3390, #16281, #17318, #18636, #5271, #5469, #18972, #1344, #8117, #5906, #21456, #13109, #11576 ) ) ;
#4408 = DIRECTION ( 'NONE',  ( 1.000000000000000000, 0.000000000000000000, -4.510774274160000731E-12 ) ) ;
#4409 = ADVANCED_FACE ( 'NONE', ( #9321 ), #18498, .F. ) ;
#4410 = AXIS2_PLACEMENT_3D ( 'NONE', #15383, #2664, #16818 ) ;
#4411 = DIRECTION ( 'NONE',  ( 1.000000000000000000, 0.000000000000000000, -2.257120985840000117E-12 ) ) ;
#4412 = CARTESIAN_POINT ( 'NONE',  ( -1.500000000000000000, 44.50000000000000000, -151.0552959529999839 ) ) ;
#4413 = FACE_OUTER_BOUND ( 'NONE', #3393, .T. ) ;
#4414 = CARTESIAN_POINT ( 'NONE',  ( -24.68734501193447883, 39.74142694379266771, -147.7937591735077376 ) ) ;
#4415 = CARTESIAN_POINT ( 'NONE',  ( 10.68320006080000084, -19.50000000000000000, -148.5552959529999839 ) ) ;
#4416 = DIRECTION ( 'NONE',  ( 1.000000000000000000, 0.000000000000000000, 0.000000000000000000 ) ) ;
#4417 = EDGE_CURVE ( 'NONE', #7697, #23331, #22730, .T. ) ;
#4418 = FACE_OUTER_BOUND ( 'NONE', #8584, .T. ) ;
#4419 = DIRECTION ( 'NONE',  ( -1.211690350419999855E-27, -2.765629237170000203E-27, 1.000000000000000000 ) ) ;
#4420 = CARTESIAN_POINT ( 'NONE',  ( -32.50000000000000000, 46.00000000000000000, -141.5552959529999839 ) ) ;
#4421 = ORIENTED_EDGE ( 'NONE', *, *, #22935, .F. ) ;
#4422 = B_SPLINE_CURVE_WITH_KNOTS ( 'NONE', 5,
 ( #3194, #10426, #12452, #21519, #14254, #12575, #7109, #8639, #15914, #5201, #23179, #10663 ),
 .UNSPECIFIED., .F., .F.,
 ( 6, 3, 3, 6 ),
 ( 0.000000000000000000, 4.398006073320000375, 8.633600727160001043, 12.71824907600000110 ),
 .UNSPECIFIED. ) ;
#4423 = CARTESIAN_POINT ( 'NONE',  ( -10.44165342908376282, 33.50172955924855955, -144.2564428470086568 ) ) ;
#4424 = DIRECTION ( 'NONE',  ( -1.526468026909999897E-13, -8.159623473500000156E-13, -1.000000000000000000 ) ) ;
#4425 = AXIS2_PLACEMENT_3D ( 'NONE', #23411, #7106, #14367 ) ;
#4426 = CARTESIAN_POINT ( 'NONE',  ( 13.13369214870000157, -50.50000000000000000, -137.0552959530000123 ) ) ;
#4427 = ORIENTED_EDGE ( 'NONE', *, *, #8857, .T. ) ;
#4428 = FACE_OUTER_BOUND ( 'NONE', #13600, .T. ) ;
#4429 = ADVANCED_FACE ( 'NONE', ( #429 ), #6216, .F. ) ;
#4430 = EDGE_CURVE ( 'NONE', #1380, #11626, #23227, .T. ) ;
#4431 = CARTESIAN_POINT ( 'NONE',  ( -21.69807436992272542, 35.58641824452431734, -147.1799120564807879 ) ) ;
#4432 = CARTESIAN_POINT ( 'NONE',  ( -9.056357402059999728, -12.43025388040000045, -147.0552959529999839 ) ) ;
#4433 = ORIENTED_EDGE ( 'NONE', *, *, #5957, .T. ) ;
#4434 = CARTESIAN_POINT ( 'NONE',  ( -22.99045472634351128, 38.45061197251095564, -140.9013473425142990 ) ) ;
#4435 = EDGE_CURVE ( 'NONE', #17995, #22397, #2458, .T. ) ;
#4436 = LINE ( 'NONE', #7762, #23034 ) ;
#4437 = EDGE_CURVE ( 'NONE', #8394, #21412, #12029, .T. ) ;
#4438 = CARTESIAN_POINT ( 'NONE',  ( 6.007375567780162129, 13.00000000000000000, -150.0552959530000123 ) ) ;
#4439 = FACE_OUTER_BOUND ( 'NONE', #2057, .T. ) ;
#4440 = FACE_OUTER_BOUND ( 'NONE', #19109, .T. ) ;
#4441 = CARTESIAN_POINT ( 'NONE',  ( -9.953901650897911679, 37.05155446197423430, -148.5872971972358698 ) ) ;
#4442 = VECTOR ( 'NONE', #19186, 1000.000000000000000 ) ;
#4443 = CARTESIAN_POINT ( 'NONE',  ( -7.965235931336511754, 40.46410429990334023, -142.0948817276852765 ) ) ;
#4444 = ORIENTED_EDGE ( 'NONE', *, *, #18967, .T. ) ;
#4445 = VECTOR ( 'NONE', #17965, 1000.000000000000000 ) ;
#4446 = CARTESIAN_POINT ( 'NONE',  ( -28.25100290369999811, 33.74243115720000219, -145.9160084049999853 ) ) ;
#4447 = FILL_AREA_STYLE_COLOUR ( '', #6174 ) ;
#4448 = VERTEX_POINT ( 'NONE', #19422 ) ;
#4449 = CARTESIAN_POINT ( 'NONE',  ( -13.69130674751348131, 32.44151991234195975, -144.7631074377568439 ) ) ;
#4450 = CARTESIAN_POINT ( 'NONE',  ( -9.873006318519999880, -23.84776512999999909, -143.5552959529999839 ) ) ;
#4451 = CARTESIAN_POINT ( 'NONE',  ( 10.68320006080000084, -19.50000000000000000, -149.3052959529999839 ) ) ;
#4452 = VERTEX_POINT ( 'NONE', #17633 ) ;
#4453 = DIRECTION ( 'NONE',  ( 0.000000000000000000, 1.000000000000000000, -2.273736754430000208E-12 ) ) ;
#4454 = CARTESIAN_POINT ( 'NONE',  ( -4.499999999969999109, 40.00000000000000000, -136.5552959530000123 ) ) ;
#4455 = ORIENTED_EDGE ( 'NONE', *, *, #15213, .F. ) ;
#4456 = DIRECTION ( 'NONE',  ( 0.000000000000000000, -1.000000000000000000, 0.000000000000000000 ) ) ;
#4457 = VECTOR ( 'NONE', #9281, 1000.000000000000114 ) ;
#4458 = EDGE_CURVE ( 'NONE', #20106, #19866, #3347, .T. ) ;
#4459 = CARTESIAN_POINT ( 'NONE',  ( -18.89556302255113707, 38.83158734770280773, -147.9443928096210641 ) ) ;
#4460 = ADVANCED_FACE ( 'NONE', ( #1108 ), #8680, .F. ) ;
#4461 =( GEOMETRIC_REPRESENTATION_CONTEXT ( 3 ) GLOBAL_UNCERTAINTY_ASSIGNED_CONTEXT ( ( #5171 ) ) GLOBAL_UNIT_ASSIGNED_CONTEXT ( ( #18238, #5138, #12863 ) ) REPRESENTATION_CONTEXT ( 'NONE', 'WORKASPACE' ) );
#4462 = CARTESIAN_POINT ( 'NONE',  ( 7.158503024131143810, 37.67301910471298498, -146.4634108040858678 ) ) ;
#4463 = LINE ( 'NONE', #15052, #2135 ) ;
#4464 = CARTESIAN_POINT ( 'NONE',  ( -24.88338928008620599, 33.38756628440417984, -141.9140409061389789 ) ) ;
#4465 = PLANE ( 'NONE',  #16974 ) ;
#4466 = ORIENTED_EDGE ( 'NONE', *, *, #21477, .T. ) ;
#4467 = DIRECTION ( 'NONE',  ( 1.526468026909999897E-13, 8.159623473500000156E-13, 1.000000000000000000 ) ) ;
#4469 = ORIENTED_EDGE ( 'NONE', *, *, #9466, .F. ) ;
#4468 = AXIS2_PLACEMENT_3D ( 'NONE', #21549, #15827, #14280 ) ;
#4470 = VERTEX_POINT ( 'NONE', #1459 ) ;
#4471 = CYLINDRICAL_SURFACE ( 'NONE', #12110, 2.999999999999999112 ) ;
#4472 = ORIENTED_EDGE ( 'NONE', *, *, #22118, .T. ) ;
#4473 = CARTESIAN_POINT ( 'NONE',  ( -10.01911575600000148, -21.69748113039999637, -148.5552959529999839 ) ) ;
#4474 = VERTEX_POINT ( 'NONE', #4669 ) ;
#4475 = ORIENTED_EDGE ( 'NONE', *, *, #19049, .F. ) ;
#4476 = DIRECTION ( 'NONE',  ( 0.000000000000000000, 0.000000000000000000, 1.000000000000000000 ) ) ;
#4477 = CARTESIAN_POINT ( 'NONE',  ( 19.00000000000000000, 33.50000000000000000, -151.0552959529999839 ) ) ;
#4478 = CARTESIAN_POINT ( 'NONE',  ( -11.58731752088923983, 38.53682247848004039, -140.5940415736972113 ) ) ;
#4479 = LINE ( 'NONE', #927, #9677 ) ;
#4480 =( BOUNDED_CURVE ( )  B_SPLINE_CURVE ( 5, ( #19726, #1410, #3545, #18056, #1769, #23061, #6746, #8989, #4973, #12221, #19496, #3190 ),
 .UNSPECIFIED., .F., .F. ) 
 B_SPLINE_CURVE_WITH_KNOTS ( ( 6, 3, 3, 6 ),
 ( 0.000000000000000000, 4.390059406679999832, 8.746277600790000051, 13.07048654050000103 ),
 .UNSPECIFIED. ) 
 CURVE ( )  GEOMETRIC_REPRESENTATION_ITEM ( )  RATIONAL_B_SPLINE_CURVE ( ( 0.2500000000000000000, 0.2500000000000000000, 0.2500000000000000000, 0.2500000000000000000, 0.2500000000000000000, 0.2500000000000000000, 0.2500000000000000000, 0.2500000000000000000, 0.2500000000000000000, 0.2500000000000000000, 0.2500000000000000000, 0.2500000000000000000 ) ) 
 REPRESENTATION_ITEM ( '' )  );
#4481 = CARTESIAN_POINT ( 'NONE',  ( -5.974012367538356294, 36.93458879463112510, -148.2930816546006270 ) ) ;
#4482 = EDGE_CURVE ( 'NONE', #5769, #14591, #6564, .T. ) ;
#4483 = CARTESIAN_POINT ( 'NONE',  ( -8.971913342289999704, 37.83624783359999810, -148.2794752869999968 ) ) ;
#4484 = ORIENTED_EDGE ( 'NONE', *, *, #23188, .F. ) ;
#4485 = B_SPLINE_CURVE_WITH_KNOTS ( 'NONE', 3,
 ( #7311, #16696, #289, #5634, #18604, #7529, #22067, #18482, #5755, #4211, #16820, #7764, #13011, #20393, #9070, #16359, #14574, #21840 ),
 .UNSPECIFIED., .F., .F.,
 ( 4, 2, 2, 2, 2, 2, 2, 2, 4 ),
 ( 0.000000000000000000, 0.1250000000000000000, 0.2500000000000000000, 0.3750000000000000000, 0.5000000000000000000, 0.6250000000000000000, 0.7500000000000000000, 0.8750000000000000000, 1.000000000000000000 ),
 .UNSPECIFIED. ) ;
#4486 = DIRECTION ( 'NONE',  ( 0.000000000000000000, 1.000000000000000000, -2.245315044999999693E-12 ) ) ;
#4487 = EDGE_CURVE ( 'NONE', #21201, #16725, #10358, .T. ) ;
#4488 = VECTOR ( 'NONE', #19047, 1000.000000000000000 ) ;
#4489 = CARTESIAN_POINT ( 'NONE',  ( 9.999986723869190186, 36.79905214429372506, -146.5552931460613877 ) ) ;
#4490 = AXIS2_PLACEMENT_3D ( 'NONE', #2010, #20076, #3898 ) ;
#4491 = CARTESIAN_POINT ( 'NONE',  ( 22.50000000000000000, 33.50000000000000000, -150.0552959529999839 ) ) ;
#4492 = ORIENTED_EDGE ( 'NONE', *, *, #6187, .F. ) ;
#4493 = CARTESIAN_POINT ( 'NONE',  ( -17.38944842999775986, 40.90832038325887510, -146.3151781682031469 ) ) ;
#4494 = DIRECTION ( 'NONE',  ( -2.507771768019999718E-12, -1.592654864069999939E-17, 1.000000000000000000 ) ) ;
#4495 = EDGE_LOOP ( 'NONE', ( #2676, #13552, #21698, #22176 ) ) ;
#4496 = CARTESIAN_POINT ( 'NONE',  ( 4.500000000009999113, -2.000000000000000000, -137.0552959530000123 ) ) ;
#4497 = ORIENTED_EDGE ( 'NONE', *, *, #7862, .T. ) ;
#4498 = LINE ( 'NONE', #11738, #8710 ) ;
#4499 = PLANE ( 'NONE',  #9185 ) ;
#4500 = ORIENTED_EDGE ( 'NONE', *, *, #4417, .T. ) ;
#4501 = CARTESIAN_POINT ( 'NONE',  ( -14.74965217825583963, 40.59671102096088191, -143.6490422507538085 ) ) ;
#4502 = CARTESIAN_POINT ( 'NONE',  ( -25.27079369000000142, 34.74837955689999802, -147.2605407199999945 ) ) ;
#4503 = ORIENTED_EDGE ( 'NONE', *, *, #14997, .F. ) ;
#4504 = CIRCLE ( 'NONE', #315, 0.5000000000000004441 ) ;
#4505 = DIRECTION ( 'NONE',  ( 0.000000000000000000, -1.000000000000000000, 0.000000000000000000 ) ) ;
#4506 = VECTOR ( 'NONE', #11252, 1000.000000000000000 ) ;
#4507 = EDGE_LOOP ( 'NONE', ( #8172, #16810, #17638, #11067 ) ) ;
#4508 = CARTESIAN_POINT ( 'NONE',  ( -31.00000000000000000, -50.00000000000000000, -149.5552959529999839 ) ) ;
#4509 = VECTOR ( 'NONE', #10927, 1000.000000000000000 ) ;
#4510 = CARTESIAN_POINT ( 'NONE',  ( -34.50000000000000000, 14.00000000000000000, -144.0552959529999839 ) ) ;
#4511 = ORIENTED_EDGE ( 'NONE', *, *, #7438, .F. ) ;
#4512 = CYLINDRICAL_SURFACE ( 'NONE', #17100, 1.499999999999999556 ) ;
#4513 = VECTOR ( 'NONE', #14501, 1000.000000000000227 ) ;
#4514 = ORIENTED_EDGE ( 'NONE', *, *, #11559, .T. ) ;
#4515 = EDGE_CURVE ( 'NONE', #7716, #22942, #12854, .T. ) ;
#4516 = AXIS2_PLACEMENT_3D ( 'NONE', #13322, #7957, #7610 ) ;
#4517 = FACE_OUTER_BOUND ( 'NONE', #13767, .T. ) ;
#4518 = CYLINDRICAL_SURFACE ( 'NONE', #23148, 3.000000000000000000 ) ;
#4519 = ADVANCED_FACE ( 'NONE', ( #8339 ), #14181, .T. ) ;
#4520 = ORIENTED_EDGE ( 'NONE', *, *, #15459, .F. ) ;
#4521 = VERTEX_POINT ( 'NONE', #21446 ) ;
#4522 = FACE_OUTER_BOUND ( 'NONE', #21064, .T. ) ;
#4523 = VECTOR ( 'NONE', #16175, 1000.000000000000000 ) ;
#4524 = CARTESIAN_POINT ( 'NONE',  ( -30.21939605167673903, 40.49321534555046043, -144.7934438824989627 ) ) ;
#4525 = VECTOR ( 'NONE', #15066, 1000.000000000000000 ) ;
#4526 = DIRECTION ( 'NONE',  ( 0.000000000000000000, 1.000000000000000000, 0.000000000000000000 ) ) ;
#4527 = CARTESIAN_POINT ( 'NONE',  ( -20.96675192182589953, -3.330829822291216047, -146.3157682189990396 ) ) ;
#4528 = VERTEX_POINT ( 'NONE', #12375 ) ;
#4529 = DIRECTION ( 'NONE',  ( 4.510774274160000731E-12, -1.321907670990000086E-13, 1.000000000000000000 ) ) ;
#4530 = DIRECTION ( 'NONE',  ( -1.000000000000000000, 0.000000000000000000, 0.000000000000000000 ) ) ;
#4531 = AXIS2_PLACEMENT_3D ( 'NONE', #21614, #14230, #1746 ) ;
#4532 = CARTESIAN_POINT ( 'NONE',  ( -13.86630785140000022, 51.50000000000000000, -136.5552959530000123 ) ) ;
#4533 = CARTESIAN_POINT ( 'NONE',  ( -10.65913935279999869, 37.04331329920000115, -139.7140392919999954 ) ) ;
#4534 = DIRECTION ( 'NONE',  ( 1.000000000000000000, 0.000000000000000000, -2.257453483404485639E-12 ) ) ;
#4535 = ORIENTED_EDGE ( 'NONE', *, *, #7925, .T. ) ;
#4536 = CARTESIAN_POINT ( 'NONE',  ( -16.62359605985811228, 34.33467835833456405, -140.1452178716700416 ) ) ;
#4537 = CARTESIAN_POINT ( 'NONE',  ( -16.72278394136257873, 36.31586521337963802, -140.5063707124225800 ) ) ;
#4538 = CARTESIAN_POINT ( 'NONE',  ( -5.371344480559407053, 37.92202225338002819, -139.4604987659717210 ) ) ;
#4539 = CARTESIAN_POINT ( 'NONE',  ( -9.157754307290000284, -15.75963164970000108, -147.5552959529999839 ) ) ;
#4540 = FACE_OUTER_BOUND ( 'NONE', #16138, .T. ) ;
#4541 = VECTOR ( 'NONE', #2541, 1000.000000000000000 ) ;
#4542 = ORIENTED_EDGE ( 'NONE', *, *, #18951, .T. ) ;
#4543 = CARTESIAN_POINT ( 'NONE',  ( -10.00627339321910370, 35.52121383151546752, -147.2841668858195305 ) ) ;
#4544 = FACE_OUTER_BOUND ( 'NONE', #8746, .T. ) ;
#4545 = CIRCLE ( 'NONE', #18979, 2.000000000000001776 ) ;
#4546 = CARTESIAN_POINT ( 'NONE',  ( 3.999999999879999546, -5.500000000000000000, -135.0552959530000123 ) ) ;
#4547 = EDGE_CURVE ( 'NONE', #23292, #16505, #16938, .T. ) ;
#4548 = ORIENTED_EDGE ( 'NONE', *, *, #1983, .T. ) ;
#4549 = VECTOR ( 'NONE', #15959, 1000.000000000000000 ) ;
#4550 = LINE ( 'NONE', #13709, #20192 ) ;
#4551 = VECTOR ( 'NONE', #21648, 1000.000000000000000 ) ;
#4552 = CIRCLE ( 'NONE', #16347, 2.999999999999999112 ) ;
#4553 = CARTESIAN_POINT ( 'NONE',  ( -29.09183339365888799, 35.07783725239920614, -139.7319361797842703 ) ) ;
#4554 = DIRECTION ( 'NONE',  ( 0.000000000000000000, 0.000000000000000000, 1.000000000000000000 ) ) ;
#4555 = ORIENTED_EDGE ( 'NONE', *, *, #8683, .F. ) ;
#4556 = CARTESIAN_POINT ( 'NONE',  ( -13.82058007329999860, 36.03909227049999942, -139.5626078809999910 ) ) ;
#4557 = FACE_OUTER_BOUND ( 'NONE', #6240, .T. ) ;
#4558 = EDGE_CURVE ( 'NONE', #15020, #3901, #1939, .T. ) ;
#4559 = CARTESIAN_POINT ( 'NONE',  ( -44.50000000000000000, 47.50000000000000000, -148.4460207619999892 ) ) ;
#4560 = PLANE ( 'NONE',  #16687 ) ;
#4561 = CARTESIAN_POINT ( 'NONE',  ( -9.779395745850974819, 34.94622798711487377, -148.4453435301223010 ) ) ;
#4562 = DIRECTION ( 'NONE',  ( 0.000000000000000000, 0.000000000000000000, 1.000000000000000000 ) ) ;
#4563 = CARTESIAN_POINT ( 'NONE',  ( 3.839256067998265465, -35.21302158184240483, -150.0552959529999839 ) ) ;
#4564 = VERTEX_POINT ( 'NONE', #14650 ) ;
#4565 = AXIS2_PLACEMENT_3D ( 'NONE', #10450, #21431, #8551 ) ;
#4566 =( NAMED_UNIT ( * ) PLANE_ANGLE_UNIT ( ) SI_UNIT ( $, .RADIAN. ) );
#4567 = EDGE_CURVE ( 'NONE', #11744, #3203, #9275, .T. ) ;
#4568 = VECTOR ( 'NONE', #5334, 1000.000000000000114 ) ;
#4569 = ORIENTED_EDGE ( 'NONE', *, *, #18194, .F. ) ;
#4570 = LINE ( 'NONE', #16833, #3878 ) ;
#4571 = CARTESIAN_POINT ( 'NONE',  ( -32.50000000000000000, 50.50000000000000000, -142.8052959529999839 ) ) ;
#4572 = ADVANCED_FACE ( 'NONE', ( #5600 ), #20127, .F. ) ;
#4573 = ORIENTED_EDGE ( 'NONE', *, *, #11887, .F. ) ;
#4574 = CARTESIAN_POINT ( 'NONE',  ( -2.499999999959999997, 40.00000000000000000, -136.0552959530000123 ) ) ;
#4575 = DIRECTION ( 'NONE',  ( 3.994014902950000436E-29, -1.000000000000000000, 4.148443855749999753E-27 ) ) ;
#4576 = ORIENTED_EDGE ( 'NONE', *, *, #7493, .T. ) ;
#4577 = CARTESIAN_POINT ( 'NONE',  ( -3.500000000000000000, 34.00000000000000000, -151.0552959529999839 ) ) ;
#4578 = CARTESIAN_POINT ( 'NONE',  ( -17.44989882367886125, 40.67283837543727998, -143.6255418396315804 ) ) ;
#4579 = VECTOR ( 'NONE', #7722, 1000.000000000000000 ) ;
#4580 = CARTESIAN_POINT ( 'NONE',  ( 7.830020039297265200, 38.34549836880493956, -146.1628100146799341 ) ) ;
#4581 = AXIS2_PLACEMENT_3D ( 'NONE', #10494, #3620, #6829 ) ;
#4582 = DIRECTION ( 'NONE',  ( 0.000000000000000000, 0.000000000000000000, 1.000000000000000000 ) ) ;
#4583 = ADVANCED_FACE ( 'NONE', ( #10819, #23455, #10709, #145, #17991, #16440 ), #7388, .F. ) ;
#4584 = CARTESIAN_POINT ( 'NONE',  ( -26.19803085470000070, 35.41001212129999942, -140.6029839040000127 ) ) ;
#4585 = CARTESIAN_POINT ( 'NONE',  ( -32.50000000000000000, 51.50000000000000000, -137.0552959530000123 ) ) ;
#4586 = ADVANCED_FACE ( 'NONE', ( #12496 ), #2053, .F. ) ;
#4587 = VERTEX_POINT ( 'NONE', #5374 ) ;
#4588 = FACE_OUTER_BOUND ( 'NONE', #22076, .T. ) ;
#4589 = ORIENTED_EDGE ( 'NONE', *, *, #22294, .T. ) ;
#4590 = CARTESIAN_POINT ( 'NONE',  ( 0.000000000000000000, 0.000000000000000000, 0.000000000000000000 ) ) ;
#4591 = EDGE_CURVE ( 'NONE', #919, #8980, #257, .T. ) ;
#4592 = VERTEX_POINT ( 'NONE', #3704 ) ;
#4593 = LINE ( 'NONE', #17319, #22016 ) ;
#4594 = EDGE_CURVE ( 'NONE', #20921, #20510, #6428, .T. ) ;
#4595 = EDGE_LOOP ( 'NONE', ( #19373, #6293, #12167, #18832 ) ) ;
#4596 = CARTESIAN_POINT ( 'NONE',  ( 1.924079216191155073, 26.46241645103238582, -136.0552959530043609 ) ) ;
#4597 = VECTOR ( 'NONE', #5076, 1000.000000000000000 ) ;
#4598 = VERTEX_POINT ( 'NONE', #8810 ) ;
#4599 = VECTOR ( 'NONE', #3774, 1000.000000000000000 ) ;
#4600 = EDGE_CURVE ( 'NONE', #15711, #1194, #22364, .T. ) ;
#4601 = ORIENTED_EDGE ( 'NONE', *, *, #3362, .T. ) ;
#4602 = LINE ( 'NONE', #11718, #15573 ) ;
#4603 = EDGE_CURVE ( 'NONE', #18727, #8753, #4504, .T. ) ;
#4604 = CARTESIAN_POINT ( 'NONE',  ( -18.48412402369122631, 36.99547888836894316, -147.4161207264432676 ) ) ;
#4605 = LINE ( 'NONE', #20671, #8067 ) ;
#4606 = FACE_OUTER_BOUND ( 'NONE', #17372, .T. ) ;
#4607 = CARTESIAN_POINT ( 'NONE',  ( -22.00705883600000234, 37.05789963359999462, -148.1619053240000028 ) ) ;
#4608 = CARTESIAN_POINT ( 'NONE',  ( 0.8371776177479999248, 12.00000000000000000, -144.0552959529999839 ) ) ;
#4609 = EDGE_LOOP ( 'NONE', ( #17653, #22994, #13312, #11168 ) ) ;
#4610 = LINE ( 'NONE', #21037, #15157 ) ;
#4611 = PRODUCT_DEFINITION_SHAPE ( 'NONE', 'NONE',  #23546 ) ;
#4612 = CARTESIAN_POINT ( 'NONE',  ( 9.960568225534427000, 37.34605842341183291, -146.5317159311745741 ) ) ;
#4613 = CARTESIAN_POINT ( 'NONE',  ( 22.89800326577686462, 33.50000000000000000, -150.0552959529999839 ) ) ;
#4614 = VECTOR ( 'NONE', #16072, 1000.000000000000114 ) ;
#4615 = EDGE_LOOP ( 'NONE', ( #11689, #18052, #484, #17711 ) ) ;
#4616 = VECTOR ( 'NONE', #20028, 1000.000000000000227 ) ;
#4617 = DIRECTION ( 'NONE',  ( -2.257144641399999941E-12, 0.000000000000000000, -1.000000000000000000 ) ) ;
#4618 = DIRECTION ( 'NONE',  ( -2.257144641399999941E-12, 0.000000000000000000, -1.000000000000000000 ) ) ;
#4619 = VERTEX_POINT ( 'NONE', #7150 ) ;
#4620 = LINE ( 'NONE', #17342, #2216 ) ;
#4621 = CARTESIAN_POINT ( 'NONE',  ( -3.499999999920000437, 34.00000000000000000, -135.0552959530000123 ) ) ;
#4622 = ORIENTED_EDGE ( 'NONE', *, *, #15648, .F. ) ;
#4623 = DIRECTION ( 'NONE',  ( 0.000000000000000000, -1.000000000000000000, -2.765629237170000203E-27 ) ) ;
#4624 = CARTESIAN_POINT ( 'NONE',  ( 7.683200060759999950, -21.50000000000000000, -143.5552959529999839 ) ) ;
#4625 = ORIENTED_EDGE ( 'NONE', *, *, #819, .F. ) ;
#4626 = CARTESIAN_POINT ( 'NONE',  ( -2.499999999959999997, 37.00000000000000000, -136.0552959530000123 ) ) ;
#4627 = APPLICATION_CONTEXT ( 'automotive_design' ) ;
#4628 = ADVANCED_FACE ( 'NONE', ( #14415 ), #7032, .T. ) ;
#4629 = CARTESIAN_POINT ( 'NONE',  ( -25.64792992843672081, 37.04465132569895758, -139.7265440088568198 ) ) ;
#4630 = ORIENTED_EDGE ( 'NONE', *, *, #2936, .T. ) ;
#4631 = SURFACE_STYLE_USAGE ( .BOTH. , #8065 ) ;
#4632 =( BOUNDED_SURFACE ( )  B_SPLINE_SURFACE ( 5, 5, ( 
 ( #10370, #1475, #8821, #15977, #6932, #19663 ),
 ( #3359, #10599, #1601, #12987, #18355, #7399 ),
 ( #18239, #14661, #11186, #16215, #7508, #21700 ),
 ( #10833, #14429, #14897, #156, #7624, #21929 ),
 ( #20021, #7163, #23467, #16558, #2064, #22155 ),
 ( #12864, #41, #5729, #12510, #19792, #5387 ),
 ( #9285, #3485, #10955, #20146, #7287, #20262 ),
 ( #14554, #8934, #3716, #10721, #1827, #14775 ),
 ( #2175, #18002, #12635, #9396, #19906, #16449 ),
 ( #3604, #3954, #1712, #3838, #1952, #5611 ),
 ( #18116, #9044, #21818, #386, #16334, #18462 ),
 ( #5502, #16672, #9172, #12749, #11075, #266 ) ),
 .UNSPECIFIED., .F., .F., .F. ) 
 B_SPLINE_SURFACE_WITH_KNOTS ( ( 6, 3, 3, 6 ),
 ( 6, 6 ),
 ( 0.000000000000000000, 4.059123295939999210, 8.340116530639999581, 12.86134770560000007 ),
 ( 0.000000000000000000, 1.570796326715864888 ),
 .UNSPECIFIED. ) 
 GEOMETRIC_REPRESENTATION_ITEM ( )  RATIONAL_B_SPLINE_SURFACE ( (
 ( 1.000000000000000000, 0.6000000000201509698, 0.4000000000201515138, 0.3000000000151135104, 0.2500000000100754960, 0.2500000000000000000),
 ( 1.000000000000000000, 0.6000000000201509698, 0.4000000000201515138, 0.3000000000151135104, 0.2500000000100754960, 0.2500000000000000000),
 ( 1.000000000000000000, 0.6000000000201509698, 0.4000000000201515138, 0.3000000000151135104, 0.2500000000100754960, 0.2500000000000000000),
 ( 1.000000000000000000, 0.6000000000201509698, 0.4000000000201515138, 0.3000000000151135104, 0.2500000000100754960, 0.2500000000000000000),
 ( 1.000000000000000000, 0.6000000000201509698, 0.4000000000201515138, 0.3000000000151135104, 0.2500000000100754960, 0.2500000000000000000),
 ( 1.000000000000000000, 0.6000000000201509698, 0.4000000000201515138, 0.3000000000151135104, 0.2500000000100754960, 0.2500000000000000000),
 ( 1.000000000000000000, 0.6000000000201509698, 0.4000000000201515138, 0.3000000000151135104, 0.2500000000100754960, 0.2500000000000000000),
 ( 1.000000000000000000, 0.6000000000201509698, 0.4000000000201515138, 0.3000000000151135104, 0.2500000000100754960, 0.2500000000000000000),
 ( 1.000000000000000000, 0.6000000000201509698, 0.4000000000201515138, 0.3000000000151135104, 0.2500000000100754960, 0.2500000000000000000),
 ( 1.000000000000000000, 0.6000000000201509698, 0.4000000000201515138, 0.3000000000151135104, 0.2500000000100754960, 0.2500000000000000000),
 ( 1.000000000000000000, 0.6000000000201509698, 0.4000000000201515138, 0.3000000000151135104, 0.2500000000100754960, 0.2500000000000000000),
 ( 1.000000000000000000, 0.6000000000201509698, 0.4000000000201515138, 0.3000000000151135104, 0.2500000000100754960, 0.2500000000000000000) ) ) 
 REPRESENTATION_ITEM ( '' )  SURFACE ( )  );
#4633 = LINE ( 'NONE', #20940, #4331 ) ;
#4634 = ORIENTED_EDGE ( 'NONE', *, *, #6385, .T. ) ;
#4635 = DIRECTION ( 'NONE',  ( 2.257144641399999941E-12, -8.049635396172279677E-35, 1.000000000000000000 ) ) ;
#4636 = PLANE ( 'NONE',  #486 ) ;
#4637 = VERTEX_POINT ( 'NONE', #3593 ) ;
#4638 = VECTOR ( 'NONE', #18546, 1000.000000000000000 ) ;
#4639 = FACE_OUTER_BOUND ( 'NONE', #17567, .T. ) ;
#4640 = CIRCLE ( 'NONE', #11074, 0.7500000000000006661 ) ;
#4641 = ORIENTED_EDGE ( 'NONE', *, *, #8554, .F. ) ;
#4642 = DIRECTION ( 'NONE',  ( -2.507771768019999718E-12, -1.592654864069999939E-17, 1.000000000000000000 ) ) ;
#4643 = CARTESIAN_POINT ( 'NONE',  ( -31.50000000000000000, 1.000000000000000000, -143.3052959529999839 ) ) ;
#4644 = EDGE_LOOP ( 'NONE', ( #23206, #11135, #22818, #8606, #7592, #15919, #14416, #23110, #294, #23197, #3430, #23172, #13316, #2699, #20994, #21859 ) ) ;
#4645 = VERTEX_POINT ( 'NONE', #1815 ) ;
#4646 = DIRECTION ( 'NONE',  ( 2.257144641399999941E-12, -4.009147065140000298E-51, 1.000000000000000000 ) ) ;
#4647 = DIRECTION ( 'NONE',  ( 2.259525899719999991E-12, 0.000000000000000000, 1.000000000000000000 ) ) ;
#4648 = DIRECTION ( 'NONE',  ( -0.9938526945756315234, 0.1107105301439589573, 0.000000000000000000 ) ) ;
#4649 = CARTESIAN_POINT ( 'NONE',  ( 31.50000000000000000, -36.53620104879999531, -136.0552959530000123 ) ) ;
#4650 = ORIENTED_EDGE ( 'NONE', *, *, #10411, .F. ) ;
#4651 = SURFACE_STYLE_USAGE ( .BOTH. , #18575 ) ;
#4652 = LINE ( 'NONE', #23090, #5895 ) ;
#4653 = VECTOR ( 'NONE', #22140, 1000.000000000000227 ) ;
#4654 = CARTESIAN_POINT ( 'NONE',  ( 23.10730091830127719, -17.50000000000000000, -150.0552959529999839 ) ) ;
#4655 = DIRECTION ( 'NONE',  ( 0.000000000000000000, 6.069065783950000909E-29, -1.000000000000000000 ) ) ;
#4656 = DIRECTION ( 'NONE',  ( -1.457881434619999915E-12, 1.723066134219999902E-12, 1.000000000000000000 ) ) ;
#4657 = EDGE_CURVE ( 'NONE', #10198, #15664, #9032, .T. ) ;
#4658 = CARTESIAN_POINT ( 'NONE',  ( -2.500000000000000000, 0.000000000000000000, -150.0552959529999839 ) ) ;
#4659 = EDGE_CURVE ( 'NONE', #6470, #20530, #7275, .T. ) ;
#4660 = VERTEX_POINT ( 'NONE', #5492 ) ;
#4661 = CARTESIAN_POINT ( 'NONE',  ( 8.250000000030000891, -39.98606797749999942, -136.0552959530000123 ) ) ;
#4662 = FACE_OUTER_BOUND ( 'NONE', #5527, .T. ) ;
#4663 = FACE_OUTER_BOUND ( 'NONE', #6718, .T. ) ;
#4664 = DIRECTION ( 'NONE',  ( -0.8571428571427679444, -0.5150787536378610421, 1.934960128632415569E-12 ) ) ;
#4665 = PLANE ( 'NONE',  #7007 ) ;
#4666 = VERTEX_POINT ( 'NONE', #10940 ) ;
#4667 = CARTESIAN_POINT ( 'NONE',  ( -10.25355660807601232, 34.02186660424427345, -142.1157150913619773 ) ) ;
#4668 = CARTESIAN_POINT ( 'NONE',  ( -31.00000000000000000, 19.50000000000000000, -149.5552959529999839 ) ) ;
#4669 = CARTESIAN_POINT ( 'NONE',  ( -27.26567793380000282, 36.96940380710000085, -148.4835048639999968 ) ) ;
#4670 =( GEOMETRIC_REPRESENTATION_CONTEXT ( 3 ) GLOBAL_UNCERTAINTY_ASSIGNED_CONTEXT ( ( #22799 ) ) GLOBAL_UNIT_ASSIGNED_CONTEXT ( ( #18007, #14559, #10726 ) ) REPRESENTATION_CONTEXT ( 'NONE', 'WORKASPACE' ) );
#4671 = ORIENTED_EDGE ( 'NONE', *, *, #14903, .F. ) ;
#4672 = CIRCLE ( 'NONE', #1649, 35.00000000000000000 ) ;
#4673 = DIRECTION ( 'NONE',  ( 2.257144641397284947E-12, -2.714724913984255017E-24, 1.000000000000000000 ) ) ;
#4674 = EDGE_CURVE ( 'NONE', #15679, #7623, #2752, .T. ) ;
#4675 = DIRECTION ( 'NONE',  ( 1.000000000000000000, 0.000000000000000000, 0.000000000000000000 ) ) ;
#4676 = ORIENTED_EDGE ( 'NONE', *, *, #16789, .T. ) ;
#4677 = CARTESIAN_POINT ( 'NONE',  ( -23.31072407292720428, 37.69002698299868115, -140.6967118636591181 ) ) ;
#4678 = CARTESIAN_POINT ( 'NONE',  ( 16.13369214859999801, 50.50000000000000000, -137.0552959530000123 ) ) ;
#4679 = CARTESIAN_POINT ( 'NONE',  ( 8.750000000030000891, -37.98606797749999942, -137.0552959530000123 ) ) ;
#4680 = LINE ( 'NONE', #15278, #7575 ) ;
#4681 = CARTESIAN_POINT ( 'NONE',  ( -9.072898850179999641, 36.94639249900000522, -148.2684494029999769 ) ) ;
#4682 = DIRECTION ( 'NONE',  ( -1.527666881879999979E-13, -8.153477892850000134E-13, -1.000000000000000000 ) ) ;
#4683 = CARTESIAN_POINT ( 'NONE',  ( -7.585922026740613333, 37.83934505584353758, -140.3341826278673636 ) ) ;
#4684 = ADVANCED_FACE ( 'NONE', ( #22374 ), #15111, .F. ) ;
#4685 = VERTEX_POINT ( 'NONE', #2403 ) ;
#4686 = PRODUCT_DEFINITION_FORMATION_WITH_SPECIFIED_SOURCE ( 'ANY', '', #13597, .NOT_KNOWN. ) ;
#4687 = EDGE_CURVE ( 'NONE', #23020, #5244, #11289, .T. ) ;
#4688 = CYLINDRICAL_SURFACE ( 'NONE', #12949, 1.500000000000001332 ) ;
#4689 = ORIENTED_EDGE ( 'NONE', *, *, #6298, .T. ) ;
#4690 = CARTESIAN_POINT ( 'NONE',  ( -6.518232409689999507, 33.41592120480000006, -146.1606736330000160 ) ) ;
#4691 = CARTESIAN_POINT ( 'NONE',  ( -29.32937220839999881, 40.41939957099999958, -140.7656299760000138 ) ) ;
#4692 = CARTESIAN_POINT ( 'NONE',  ( -21.71608528380000180, -1.500000000000000000, -146.3157682190000060 ) ) ;
#4693 = ORIENTED_EDGE ( 'NONE', *, *, #20534, .T. ) ;
#4694 = DIRECTION ( 'NONE',  ( -2.257144641399999941E-12, 8.049635416090000264E-35, -1.000000000000000000 ) ) ;
#4695 = DIRECTION ( 'NONE',  ( 1.526468026909999897E-13, 8.159623473500000156E-13, 1.000000000000000000 ) ) ;
#4696 = ORIENTED_EDGE ( 'NONE', *, *, #21770, .F. ) ;
#4697 = CARTESIAN_POINT ( 'NONE',  ( -21.97930707628684033, 37.84604761964991582, -147.8229183002398770 ) ) ;
#4698 = CARTESIAN_POINT ( 'NONE',  ( -17.37084003756964279, 38.37330577533303710, -140.8480132324181966 ) ) ;
#4699 = CARTESIAN_POINT ( 'NONE',  ( 3.611212474210000402E-11, 0.000000000000000000, -135.0552959530000123 ) ) ;
#4700 = CARTESIAN_POINT ( 'NONE',  ( 7.156500972566314012, 36.32574979380856206, -146.4644491674769426 ) ) ;
#4701 = ADVANCED_FACE ( 'NONE', ( #2627 ), #22606, .T. ) ;
#4702 = LINE ( 'NONE', #10622, #15791 ) ;
#4703 = CARTESIAN_POINT ( 'NONE',  ( -24.39503929831862195, 33.43607675443129068, -146.0584967254518460 ) ) ;
#4704 = CARTESIAN_POINT ( 'NONE',  ( 29.68320006080000084, -16.50000000000000000, -150.0552959529999839 ) ) ;
#4705 = CARTESIAN_POINT ( 'NONE',  ( -10.97748938910000049, 39.75689975739999937, -140.4868351200000234 ) ) ;
#4706 = VERTEX_POINT ( 'NONE', #9733 ) ;
#4707 = PLANE ( 'NONE',  #22344 ) ;
#4708 = EDGE_CURVE ( 'NONE', #19961, #22823, #14996, .T. ) ;
#4709 = VERTEX_POINT ( 'NONE', #6299 ) ;
#4710 = EDGE_LOOP ( 'NONE', ( #19752, #17367, #20755, #19476 ) ) ;
#4711 = DIRECTION ( 'NONE',  ( 0.9999976651796518290, -0.002160933882609249439, -8.955304954746877373E-12 ) ) ;
#4712 = ORIENTED_EDGE ( 'NONE', *, *, #4133, .T. ) ;
#4713 = LINE ( 'NONE', #4831, #340 ) ;
#4714 = ORIENTED_EDGE ( 'NONE', *, *, #17217, .F. ) ;
#4715 = ORIENTED_EDGE ( 'NONE', *, *, #10137, .T. ) ;
#4716 = AXIS2_PLACEMENT_3D ( 'NONE', #17031, #11544, #9405 ) ;
#4717 = CARTESIAN_POINT ( 'NONE',  ( -34.50000000000000000, 26.00000000000000000, -150.5552959529999839 ) ) ;
#4718 = ADVANCED_FACE ( 'NONE', ( #7612 ), #22258, .T. ) ;
#4719 = CARTESIAN_POINT ( 'NONE',  ( -18.91006587269999883, 33.19603641719999843, -143.7906546520000006 ) ) ;
#4720 = CARTESIAN_POINT ( 'NONE',  ( -10.64004713443764061, 38.83279341006178953, -140.2200294818480302 ) ) ;
#4721 = FACE_OUTER_BOUND ( 'NONE', #16269, .T. ) ;
#4722 = CARTESIAN_POINT ( 'NONE',  ( -8.554523812450000264, 40.80811760249999764, -146.2789059460000090 ) ) ;
#4723 = EDGE_LOOP ( 'NONE', ( #13185, #9735, #15541, #19053 ) ) ;
#4724 = FACE_OUTER_BOUND ( 'NONE', #6257, .T. ) ;
#4725 = EDGE_CURVE ( 'NONE', #12052, #13585, #3352, .T. ) ;
#4726 = CARTESIAN_POINT ( 'NONE',  ( 9.412671590450063519, 35.80533467859499552, -146.2522312778014282 ) ) ;
#4727 = ADVANCED_FACE ( 'NONE', ( #11411 ), #18449, .T. ) ;
#4728 = DIRECTION ( 'NONE',  ( 0.000000000000000000, 0.000000000000000000, 1.000000000000000000 ) ) ;
#4729 = ORIENTED_EDGE ( 'NONE', *, *, #11781, .T. ) ;
#4730 = EDGE_CURVE ( 'NONE', #21289, #8120, #9386, .T. ) ;
#4731 = CIRCLE ( 'NONE', #21461, 0.7500000000000006661 ) ;
#4732 = EDGE_CURVE ( 'NONE', #4332, #751, #22497, .T. ) ;
#4733 = CARTESIAN_POINT ( 'NONE',  ( -30.47299999999999898, 12.24483487620000055, -145.0141470300000037 ) ) ;
#4734 = CARTESIAN_POINT ( 'NONE',  ( 18.18320006080000084, -3.000000000000000000, -150.0552959529999839 ) ) ;
#4735 = VERTEX_POINT ( 'NONE', #22144 ) ;
#4736 = FACE_OUTER_BOUND ( 'NONE', #23383, .T. ) ;
#4737 = ORIENTED_EDGE ( 'NONE', *, *, #19081, .T. ) ;
#4738 = DIRECTION ( 'NONE',  ( -0.6427876096862108479, 0.000000000000000000, -0.7660444431192537929 ) ) ;
#4739 = CARTESIAN_POINT ( 'NONE',  ( -6.683153925719999222, -51.50000000000000000, -136.0552959530000123 ) ) ;
#4740 = EDGE_LOOP ( 'NONE', ( #14376, #15588, #9277, #4874, #16642, #930, #11341 ) ) ;
#4741 = DIRECTION ( 'NONE',  ( 0.000000000000000000, 0.000000000000000000, -1.000000000000000000 ) ) ;
#4742 = CARTESIAN_POINT ( 'NONE',  ( -25.91593243209636199, 32.87307245982592718, -143.7099744806644139 ) ) ;
#4743 = ORIENTED_EDGE ( 'NONE', *, *, #20662, .T. ) ;
#4744 = PLANE ( 'NONE',  #10393 ) ;
#4745 = ORIENTED_EDGE ( 'NONE', *, *, #19694, .F. ) ;
#4746 = DIRECTION ( 'NONE',  ( 1.000000000000000000, 0.000000000000000000, -2.257120985840000117E-12 ) ) ;
#4747 = CYLINDRICAL_SURFACE ( 'NONE', #16812, 35.00000000000000000 ) ;
#4748 = ORIENTED_EDGE ( 'NONE', *, *, #5602, .F. ) ;
#4749 = LINE ( 'NONE', #2851, #17077 ) ;
#4750 = VERTEX_POINT ( 'NONE', #20360 ) ;
#4751 = DIRECTION ( 'NONE',  ( 4.430233957459999899E-12, -6.110667527539999876E-13, 1.000000000000000000 ) ) ;
#4752 = CARTESIAN_POINT ( 'NONE',  ( -24.79371418840000274, 32.62011804889999667, -144.5039952340000013 ) ) ;
#4753 = AXIS2_PLACEMENT_3D ( 'NONE', #17014, #2632, #9862 ) ;
#4754 = VERTEX_POINT ( 'NONE', #4054 ) ;
#4755 = B_SPLINE_CURVE_WITH_KNOTS ( 'NONE', 3,
 ( #16119, #5161, #17778, #7185, #10281, #19461, #17553, #1270, #3265, #8493, #14097, #17905, #15763, #12407, #10391, #17665, #1374, #5058 ),
 .UNSPECIFIED., .F., .F.,
 ( 4, 2, 2, 2, 2, 2, 2, 2, 4 ),
 ( 0.000000000000000000, 0.1250000000000000000, 0.2500000000000000000, 0.3750000000000000000, 0.5000000000000000000, 0.6250000000000000000, 0.7500000000000000000, 0.8750000000000000000, 1.000000000000000000 ),
 .UNSPECIFIED. ) ;
#4756 = EDGE_CURVE ( 'NONE', #19035, #777, #18565, .T. ) ;
#4757 = EDGE_CURVE ( 'NONE', #17568, #9722, #13324, .T. ) ;
#4758 = ORIENTED_EDGE ( 'NONE', *, *, #9236, .F. ) ;
#4759 = DIRECTION ( 'NONE',  ( -0.7071067811865471286, 0.7071067811865477948, 1.595945597898661113E-12 ) ) ;
#4760 = DIRECTION ( 'NONE',  ( 0.000000000000000000, 1.000000000000000000, 0.000000000000000000 ) ) ;
#4761 = CARTESIAN_POINT ( 'NONE',  ( -14.70777071217397314, 41.11523651854984962, -146.4493477498343168 ) ) ;
#4762 = CARTESIAN_POINT ( 'NONE',  ( -9.999999999959999997, 48.50000000000000000, -136.0552959530000123 ) ) ;
#4763 = ORIENTED_EDGE ( 'NONE', *, *, #2885, .F. ) ;
#4764 =( NAMED_UNIT ( * ) PLANE_ANGLE_UNIT ( ) SI_UNIT ( $, .RADIAN. ) );
#4765 = CARTESIAN_POINT ( 'NONE',  ( 4.999999999879999990, -4.750000000000000000, -135.4552959529999896 ) ) ;
#4766 =( BOUNDED_SURFACE ( )  B_SPLINE_SURFACE ( 5, 5, ( 
 ( #9375, #11514, #3819, #5822, #18681, #5940 ),
 ( #22363, #18791, #20465, #4046, #14986, #14750 ),
 ( #22247, #12964, #13192, #11399, #2502, #2394 ),
 ( #11054, #13314, #20242, #12840, #11169, #9614 ),
 ( #596, #21909, #9724, #5591, #18441, #9267 ),
 ( #2156, #16999, #16538, #6062, #16887, #14877 ),
 ( #16011, #13987, #13426, #19701, #5176, #8507 ),
 ( #6178, #3395, #8612, #10637, #21259, #12076 ),
 ( #17918, #23276, #1635, #4955, #12199, #6966 ),
 ( #17122, #12424, #14231, #19588, #20695, #19350 ),
 ( #4388, #8396, #15230, #2613, #22484, #11627 ),
 ( #18903, #15777, #17794, #23154, #23039, #6611 ) ),
 .UNSPECIFIED., .F., .F., .F. ) 
 B_SPLINE_SURFACE_WITH_KNOTS ( ( 6, 3, 3, 6 ),
 ( 6, 6 ),
 ( 0.000000000000000000, 4.564346237179999655, 9.066392868600001265, 13.51003987140000007 ),
 ( 1.570796326695754974, 3.141592653590000062 ),
 .UNSPECIFIED. ) 
 GEOMETRIC_REPRESENTATION_ITEM ( )  RATIONAL_B_SPLINE_SURFACE ( (
 ( 0.2500000000000000000, 0.2499999999873634970, 0.2999999999810455398, 0.3999999999747270163, 0.5999999999747269719, 1.000000000000000000),
 ( 0.2500000000000000000, 0.2499999999873634970, 0.2999999999810455398, 0.3999999999747270163, 0.5999999999747269719, 1.000000000000000000),
 ( 0.2500000000000000000, 0.2499999999873634970, 0.2999999999810455398, 0.3999999999747270163, 0.5999999999747269719, 1.000000000000000000),
 ( 0.2500000000000000000, 0.2499999999873634970, 0.2999999999810455398, 0.3999999999747270163, 0.5999999999747269719, 1.000000000000000000),
 ( 0.2500000000000000000, 0.2499999999873634970, 0.2999999999810455398, 0.3999999999747270163, 0.5999999999747269719, 1.000000000000000000),
 ( 0.2500000000000000000, 0.2499999999873634970, 0.2999999999810455398, 0.3999999999747270163, 0.5999999999747269719, 1.000000000000000000),
 ( 0.2500000000000000000, 0.2499999999873634970, 0.2999999999810455398, 0.3999999999747270163, 0.5999999999747269719, 1.000000000000000000),
 ( 0.2500000000000000000, 0.2499999999873634970, 0.2999999999810455398, 0.3999999999747270163, 0.5999999999747269719, 1.000000000000000000),
 ( 0.2500000000000000000, 0.2499999999873634970, 0.2999999999810455398, 0.3999999999747270163, 0.5999999999747269719, 1.000000000000000000),
 ( 0.2500000000000000000, 0.2499999999873634970, 0.2999999999810455398, 0.3999999999747270163, 0.5999999999747269719, 1.000000000000000000),
 ( 0.2500000000000000000, 0.2499999999873634970, 0.2999999999810455398, 0.3999999999747270163, 0.5999999999747269719, 1.000000000000000000),
 ( 0.2500000000000000000, 0.2499999999873634970, 0.2999999999810455398, 0.3999999999747270163, 0.5999999999747269719, 1.000000000000000000) ) ) 
 REPRESENTATION_ITEM ( '' )  SURFACE ( )  );
#4768 = CARTESIAN_POINT ( 'NONE',  ( 20.87864083493722234, -18.98914305888730425, -150.0552959529999839 ) ) ;
#4767 = B_SPLINE_CURVE_WITH_KNOTS ( 'NONE', 3,
 ( #6431, #972, #15124, #8324, #20717, #13449, #2870, #9634, #19281, #17377, #16907, #15600, #8205, #15250, #6312, #13817, #6087, #2640 ),
 .UNSPECIFIED., .F., .F.,
 ( 4, 2, 2, 2, 2, 2, 2, 2, 4 ),
 ( 0.000000000000000000, 0.1249999999999998335, 0.2499999999999996669, 0.3749999999999995004, 0.4999999999999993339, 0.6250000000000002220, 0.7500000000000002220, 0.8750000000000001110, 1.000000000000000000 ),
 .UNSPECIFIED. ) ;
#4769 = DIRECTION ( 'NONE',  ( 4.510774274160000731E-12, -1.321907670990000086E-13, 1.000000000000000000 ) ) ;
#4770 = FACE_OUTER_BOUND ( 'NONE', #22126, .T. ) ;
#4771 = CARTESIAN_POINT ( 'NONE',  ( 8.750000000000000000, -47.00000000000000000, -150.0552959529999839 ) ) ;
#4772 = VECTOR ( 'NONE', #6547, 1000.000000000000000 ) ;
#4773 = AXIS2_PLACEMENT_3D ( 'NONE', #12684, #92, #12915 ) ;
#4774 = VERTEX_POINT ( 'NONE', #16895 ) ;
#4775 = CARTESIAN_POINT ( 'NONE',  ( -31.00000000000000000, -51.50000000000000000, -149.5552959529999839 ) ) ;
#4776 = DIRECTION ( 'NONE',  ( 2.255973186040000320E-12, 0.000000000000000000, 1.000000000000000000 ) ) ;
#4777 = LINE ( 'NONE', #17271, #2745 ) ;
#4778 = LINE ( 'NONE', #20725, #9925 ) ;
#4779 = DIRECTION ( 'NONE',  ( 0.000000000000000000, -1.000000000000000000, 0.000000000000000000 ) ) ;
#4780 = ORIENTED_EDGE ( 'NONE', *, *, #18061, .T. ) ;
#4781 = LINE ( 'NONE', #3006, #20519 ) ;
#4782 = CARTESIAN_POINT ( 'NONE',  ( -6.683153925719999222, 50.50000000000000000, -149.5552959529999839 ) ) ;
#4783 = CARTESIAN_POINT ( 'NONE',  ( -26.39607007120000048, 36.95534867429999792, -140.3840478969999879 ) ) ;
#4784 = ORIENTED_EDGE ( 'NONE', *, *, #10976, .F. ) ;
#4785 = PRODUCT ( 'Main Base', 'Main Base', '', ( #23379 ) ) ;
#4786 = EDGE_CURVE ( 'NONE', #4356, #16880, #3596, .T. ) ;
#4788 = CARTESIAN_POINT ( 'NONE',  ( -29.62827070405596430, 36.92763176543257941, -139.7399851633785488 ) ) ;
#4787 = AXIS2_PLACEMENT_3D ( 'NONE', #1538, #21638, #8877 ) ;
#4789 = CIRCLE ( 'NONE', #2522, 0.7500000000000006661 ) ;
#4790 = FACE_OUTER_BOUND ( 'NONE', #3662, .T. ) ;
#4791 = ORIENTED_EDGE ( 'NONE', *, *, #23482, .T. ) ;
#4792 = CARTESIAN_POINT ( 'NONE',  ( -22.83308877303491968, 39.55027303352079571, -140.7145628013014118 ) ) ;
#4793 = DIRECTION ( 'NONE',  ( 1.000000000000000000, 0.000000000000000000, -4.511206223393553012E-12 ) ) ;
#4794 = DIRECTION ( 'NONE',  ( 1.000000000000000000, 0.000000000000000000, 0.000000000000000000 ) ) ;
#4795 = DIRECTION ( 'NONE',  ( 2.257144641404620116E-12, 2.777754792983395132E-24, 1.000000000000000000 ) ) ;
#4796 = ORIENTED_EDGE ( 'NONE', *, *, #3201, .F. ) ;
#4797 = CARTESIAN_POINT ( 'NONE',  ( -10.28060652843288025, 34.62853500624063940, -147.1732277804927946 ) ) ;
#4798 = CARTESIAN_POINT ( 'NONE',  ( 7.000000000050000004, 37.00000000000000000, -146.5552959529999839 ) ) ;
#4799 = CARTESIAN_POINT ( 'NONE',  ( 9.479581287884620622, -37.28079462196955518, -150.0552959529999839 ) ) ;
#4800 = DIRECTION ( 'NONE',  ( -1.000000000000000000, 0.000000000000000000, 2.245315044999999693E-12 ) ) ;
#4801 = ORIENTED_EDGE ( 'NONE', *, *, #23402, .F. ) ;
#4802 = SURFACE_STYLE_FILL_AREA ( #19445 ) ;
#4803 = SURFACE_SIDE_STYLE ('',( #17534 ) ) ;
#4804 = ORIENTED_EDGE ( 'NONE', *, *, #16069, .F. ) ;
#4805 = VECTOR ( 'NONE', #21719, 1000.000000000000000 ) ;
#4806 = CARTESIAN_POINT ( 'NONE',  ( -6.284562654584142649, 35.48787867574768029, -147.4335637949685065 ) ) ;
#4807 = CARTESIAN_POINT ( 'NONE',  ( -25.74743564699999965, 37.94517732370000118, -139.7356315989999871 ) ) ;
#4808 = AXIS2_PLACEMENT_3D ( 'NONE', #4, #12713, #11043 ) ;
#4809 = CARTESIAN_POINT ( 'NONE',  ( 16.82730212879999598, -31.88969284570000084, -145.5552959529999839 ) ) ;
#4810 = EDGE_LOOP ( 'NONE', ( #19167, #14249, #3607, #21619 ) ) ;
#4811 = DIRECTION ( 'NONE',  ( 0.000000000000000000, 0.000000000000000000, 1.000000000000000000 ) ) ;
#4812 = CARTESIAN_POINT ( 'NONE',  ( -34.50000000000000000, 76.00000000000000000, -155.5552959529999839 ) ) ;
#4813 = ORIENTED_EDGE ( 'NONE', *, *, #12596, .F. ) ;
#4814 = DIRECTION ( 'NONE',  ( -2.507771768019999718E-12, -1.592654864069999939E-17, 1.000000000000000000 ) ) ;
#4815 = EDGE_CURVE ( 'NONE', #21392, #5806, #2226, .T. ) ;
#4816 = CARTESIAN_POINT ( 'NONE',  ( -17.97686571119999854, 41.53571570570000659, -143.4577736070000071 ) ) ;
#4817 = CARTESIAN_POINT ( 'NONE',  ( -13.48914305888730425, -40.37864083493721523, -150.0552959529999839 ) ) ;
#4818 = ADVANCED_FACE ( 'NONE', ( #8309 ), #23079, .F. ) ;
#4819 = DIRECTION ( 'NONE',  ( 0.000000000000000000, -1.000000000000000000, 0.000000000000000000 ) ) ;
#4820 = DIRECTION ( 'NONE',  ( -1.000000000000000000, 0.000000000000000000, 2.257221436789999912E-12 ) ) ;
#4821 = CIRCLE ( 'NONE', #2551, 1.499999999999999556 ) ;
#4822 = CARTESIAN_POINT ( 'NONE',  ( -25.28614709708956809, 36.22712742843352629, -140.0123646937360036 ) ) ;
#4823 = LINE ( 'NONE', #19336, #2921 ) ;
#4824 = DIRECTION ( 'NONE',  ( 1.000000000000000000, 0.000000000000000000, -2.259525899719999991E-12 ) ) ;
#4825 = VERTEX_POINT ( 'NONE', #19397 ) ;
#4826 = CARTESIAN_POINT ( 'NONE',  ( -23.81889237380000068, 39.38287674749999923, -140.7489234159999967 ) ) ;
#4827 = EDGE_LOOP ( 'NONE', ( #52, #95, #4469, #11592 ) ) ;
#4828 = PRESENTATION_STYLE_ASSIGNMENT (( #16008 ) ) ;
#4829 = EDGE_LOOP ( 'NONE', ( #8714, #3802, #14735, #6395 ) ) ;
#4830 = ORIENTED_EDGE ( 'NONE', *, *, #16022, .F. ) ;
#4831 = CARTESIAN_POINT ( 'NONE',  ( -32.50000000000000000, -50.50000000000000000, -143.0552959529999839 ) ) ;
#4832 = LINE ( 'NONE', #10293, #18689 ) ;
#4833 = ORIENTED_EDGE ( 'NONE', *, *, #19853, .T. ) ;
#4834 = AXIS2_PLACEMENT_3D ( 'NONE', #14100, #23492, #17781 ) ;
#4835 = ORIENTED_EDGE ( 'NONE', *, *, #57, .F. ) ;
#4836 = DIRECTION ( 'NONE',  ( 0.000000000000000000, 0.000000000000000000, -1.000000000000000000 ) ) ;
#4837 = CARTESIAN_POINT ( 'NONE',  ( -9.870393330389999775, 37.85345449830000319, -147.8311166189999994 ) ) ;
#4838 = FACE_OUTER_BOUND ( 'NONE', #20075, .T. ) ;
#4839 = CARTESIAN_POINT ( 'NONE',  ( -10.00000000000000000, 25.50000000000000000, -151.0552959529999839 ) ) ;
#4840 = CARTESIAN_POINT ( 'NONE',  ( -7.324031428439999658, 35.31041870520000003, -140.2046280479999893 ) ) ;
#4841 = FACE_OUTER_BOUND ( 'NONE', #21996, .T. ) ;
#4842 = EDGE_LOOP ( 'NONE', ( #20125, #22858, #14646, #16712 ) ) ;
#4843 = DIRECTION ( 'NONE',  ( 1.000000000000000000, 0.000000000000000000, -8.955190032050000935E-12 ) ) ;
#4844 = EDGE_CURVE ( 'NONE', #13274, #18962, #6766, .T. ) ;
#4845 = DIRECTION ( 'NONE',  ( 0.7071067811865474617, 0.7071067811865476838, -1.595020412044806951E-12 ) ) ;
#4846 = PLANE ( 'NONE',  #19359 ) ;
#4847 = ORIENTED_EDGE ( 'NONE', *, *, #23519, .T. ) ;
#4848 = AXIS2_PLACEMENT_3D ( 'NONE', #828, #7314, #14335 ) ;
#4849 = EDGE_CURVE ( 'NONE', #16183, #18180, #22559, .T. ) ;
#4850 = DIRECTION ( 'NONE',  ( 0.000000000000000000, 0.000000000000000000, 1.000000000000000000 ) ) ;
#4851 = VECTOR ( 'NONE', #16760, 1000.000000000000000 ) ;
#4852 = VERTEX_POINT ( 'NONE', #10213 ) ;
#4853 = DIRECTION ( 'NONE',  ( -1.000000000000000000, 0.000000000000000000, 2.257495777610000006E-12 ) ) ;
#4854 = CARTESIAN_POINT ( 'NONE',  ( -3.500000048370000005, 34.80604359529999670, -142.8567321060000097 ) ) ;
#4855 = ORIENTED_EDGE ( 'NONE', *, *, #23082, .T. ) ;
#4856 = CARTESIAN_POINT ( 'NONE',  ( -23.51619327739999932, 36.94101002280000046, -140.1031831869999849 ) ) ;
#4857 = CARTESIAN_POINT ( 'NONE',  ( 6.000000000000000000, -3.500000000000000000, -150.0552959529999839 ) ) ;
#4858 = ORIENTED_EDGE ( 'NONE', *, *, #16935, .T. ) ;
#4859 = CARTESIAN_POINT ( 'NONE',  ( -15.43367019712668053, 41.39476109361318379, -144.4317641176221798 ) ) ;
#4860 = CARTESIAN_POINT ( 'NONE',  ( -25.90907760989742670, 37.01347911741230945, -139.4251635482865765 ) ) ;
#4861 = ORIENTED_EDGE ( 'NONE', *, *, #8433, .T. ) ;
#4862 =( NAMED_UNIT ( * ) PLANE_ANGLE_UNIT ( ) SI_UNIT ( $, .RADIAN. ) );
#4863 = EDGE_CURVE ( 'NONE', #19147, #11046, #21301, .T. ) ;
#4864 = EDGE_LOOP ( 'NONE', ( #4925, #11199, #15718 ) ) ;
#4865 = FACE_OUTER_BOUND ( 'NONE', #5562, .T. ) ;
#4866 = FACE_OUTER_BOUND ( 'NONE', #253, .T. ) ;
#4867 = VERTEX_POINT ( 'NONE', #12118 ) ;
#4868 = LINE ( 'NONE', #14026, #7583 ) ;
#4869 = EDGE_CURVE ( 'NONE', #2277, #824, #15934, .T. ) ;
#4870 = AXIS2_PLACEMENT_3D ( 'NONE', #7510, #10956, #13214 ) ;
#4871 = DIRECTION ( 'NONE',  ( 0.000000000000000000, 1.000000000000000000, 0.000000000000000000 ) ) ;
#4872 = AXIS2_PLACEMENT_3D ( 'NONE', #5169, #12870, #23150 ) ;
#4873 = CARTESIAN_POINT ( 'NONE',  ( -1.499999999960000219, 44.50000000000000000, -136.0552959530000123 ) ) ;
#4874 = ORIENTED_EDGE ( 'NONE', *, *, #21808, .F. ) ;
#4875 = DIRECTION ( 'NONE',  ( -1.527666881879999979E-13, -8.171241461240000022E-13, -1.000000000000000000 ) ) ;
#4876 = ADVANCED_FACE ( 'NONE', ( #6538 ), #17485, .T. ) ;
#4877 = CARTESIAN_POINT ( 'NONE',  ( -14.74521098486907889, 37.74183931348511578, -147.9812505911391156 ) ) ;
#4878 = CARTESIAN_POINT ( 'NONE',  ( -31.00000000000000000, 0.000000000000000000, -151.0552959529999839 ) ) ;
#4879 = ORIENTED_EDGE ( 'NONE', *, *, #11258, .F. ) ;
#4880 = CARTESIAN_POINT ( 'NONE',  ( -22.10824191589999899, -4.000000000000000000, -145.5657682190000060 ) ) ;
#4881 = CARTESIAN_POINT ( 'NONE',  ( -2.499999999959999997, 37.00000000000000000, -153.0552959529999839 ) ) ;
#4882 = ADVANCED_FACE ( 'NONE', ( #20823 ), #4518, .T. ) ;
#4883 = AXIS2_PLACEMENT_3D ( 'NONE', #16546, #10583, #11063 ) ;
#4884 = DIRECTION ( 'NONE',  ( 2.839308199620000013E-14, 3.568879590630000244E-13, 1.000000000000000000 ) ) ;
#4885 = LINE ( 'NONE', #17621, #301 ) ;
#4886 = LINE ( 'NONE', #867, #16775 ) ;
#4887 = DIRECTION ( 'NONE',  ( -2.602084747547159675E-17, 1.000000000000000000, 2.714790849608250461E-29 ) ) ;
#4888 = VECTOR ( 'NONE', #18677, 1000.000000000000000 ) ;
#4889 = VERTEX_POINT ( 'NONE', #960 ) ;
#4890 = CARTESIAN_POINT ( 'NONE',  ( -16.15855174276306272, 35.42854167619758954, -140.1130648018951206 ) ) ;
#4891 = ADVANCED_FACE ( 'NONE', ( #21067 ), #12002, .T. ) ;
#4892 = AXIS2_PLACEMENT_3D ( 'NONE', #9352, #7810, #20219 ) ;
#4893 = DIRECTION ( 'NONE',  ( 0.1720749717299729364, 0.9850838563818457017, -6.484322019408987829E-13 ) ) ;
#4894 = EDGE_CURVE ( 'NONE', #5505, #18280, #2856, .T. ) ;
#4895 = CARTESIAN_POINT ( 'NONE',  ( 1.172620240290000115, -63.19354141059999108, -145.5552959529999839 ) ) ;
#4896 = CARTESIAN_POINT ( 'NONE',  ( -24.30767937719999949, 40.97374044589999897, -144.4830919949999952 ) ) ;
#4897 = CARTESIAN_POINT ( 'NONE',  ( -12.50000000000000000, 19.50000000000000000, -150.0552959529999839 ) ) ;
#4898 = EDGE_CURVE ( 'NONE', #6741, #11959, #5656, .T. ) ;
#4899 = VERTEX_POINT ( 'NONE', #10333 ) ;
#4900 = DIRECTION ( 'NONE',  ( 1.000000000000000000, 0.000000000000000000, 0.000000000000000000 ) ) ;
#4901 = CARTESIAN_POINT ( 'NONE',  ( 4.698575659221273071, -2.000067229902509514, -150.0552959529999839 ) ) ;
#4902 = ORIENTED_EDGE ( 'NONE', *, *, #20300, .T. ) ;
#4903 = VECTOR ( 'NONE', #5788, 1000.000000000000000 ) ;
#4904 = CARTESIAN_POINT ( 'NONE',  ( -28.85277900879999891, 34.87340808660000135, -141.1101275619999740 ) ) ;
#4905 = CARTESIAN_POINT ( 'NONE',  ( 8.500000000060001781, 38.50000000000000000, -146.0552959529999839 ) ) ;
#4906 = ORIENTED_EDGE ( 'NONE', *, *, #4304, .T. ) ;
#4907 =( BOUNDED_SURFACE ( )  B_SPLINE_SURFACE ( 5, 5, ( 
 ( #18371, #19924, #7309, #21837, #7526, #20041 ),
 ( #5632, #5520, #12769, #20277, #2192, #10072 ),
 ( #21055, #1310, #12105, #2735, #6284, #13540 ),
 ( #4502, #17351, #6640, #4981, #8424, #21288 ),
 ( #19503, #15339, #22707, #9962, #3197, #11986 ),
 ( #10429, #10322, #6525, #10196, #19141, #1064 ),
 ( #11871, #4742, #15446, #8532, #22595, #838 ),
 ( #19382, #19251, #6754, #14016, #17471, #6400 ),
 ( #20937, #13902, #2964, #15570, #1196, #20811 ),
 ( #15805, #8061, #15694, #11743, #8295, #19024 ),
 ( #17235, #22957, #22835, #946, #21174, #13793 ),
 ( #3088, #8174, #23069, #13662, #4860, #4629 ) ),
 .UNSPECIFIED., .F., .F., .F. ) 
 B_SPLINE_SURFACE_WITH_KNOTS ( ( 6, 3, 3, 6 ),
 ( 6, 6 ),
 ( 0.000000000000000000, 4.454241660750000165, 8.943513424000000711, 13.47090878500000066 ),
 ( 0.000000000000000000, 1.570796327036555029 ),
 .UNSPECIFIED. ) 
 GEOMETRIC_REPRESENTATION_ITEM ( )  RATIONAL_B_SPLINE_SURFACE ( (
 ( 1.000000000000000000, 0.5999999999384889593, 0.3999999999384890037, 0.2999999999538665030, 0.2499999999692444907, 0.2500000000000000000),
 ( 1.000000000000000000, 0.5999999999384889593, 0.3999999999384890037, 0.2999999999538665030, 0.2499999999692444907, 0.2500000000000000000),
 ( 1.000000000000000000, 0.5999999999384889593, 0.3999999999384890037, 0.2999999999538665030, 0.2499999999692444907, 0.2500000000000000000),
 ( 1.000000000000000000, 0.5999999999384889593, 0.3999999999384890037, 0.2999999999538665030, 0.2499999999692444907, 0.2500000000000000000),
 ( 1.000000000000000000, 0.5999999999384889593, 0.3999999999384890037, 0.2999999999538665030, 0.2499999999692444907, 0.2500000000000000000),
 ( 1.000000000000000000, 0.5999999999384889593, 0.3999999999384890037, 0.2999999999538665030, 0.2499999999692444907, 0.2500000000000000000),
 ( 1.000000000000000000, 0.5999999999384889593, 0.3999999999384890037, 0.2999999999538665030, 0.2499999999692444907, 0.2500000000000000000),
 ( 1.000000000000000000, 0.5999999999384889593, 0.3999999999384890037, 0.2999999999538665030, 0.2499999999692444907, 0.2500000000000000000),
 ( 1.000000000000000000, 0.5999999999384889593, 0.3999999999384890037, 0.2999999999538665030, 0.2499999999692444907, 0.2500000000000000000),
 ( 1.000000000000000000, 0.5999999999384889593, 0.3999999999384890037, 0.2999999999538665030, 0.2499999999692444907, 0.2500000000000000000),
 ( 1.000000000000000000, 0.5999999999384889593, 0.3999999999384890037, 0.2999999999538665030, 0.2499999999692444907, 0.2500000000000000000),
 ( 1.000000000000000000, 0.5999999999384889593, 0.3999999999384890037, 0.2999999999538665030, 0.2499999999692444907, 0.2500000000000000000) ) ) 
 REPRESENTATION_ITEM ( '' )  SURFACE ( )  );
#4908 = AXIS2_PLACEMENT_3D ( 'NONE', #10933, #16313, #3464 ) ;
#4909 = CARTESIAN_POINT ( 'NONE',  ( -23.65394330256869182, 40.08423268064209566, -145.9325622199873465 ) ) ;
#4910 = DIRECTION ( 'NONE',  ( 1.000000000000000000, 0.000000000000000000, 2.507771768019999718E-12 ) ) ;
#4911 = VECTOR ( 'NONE', #17103, 1000.000000000000000 ) ;
#4912 = DIRECTION ( 'NONE',  ( 0.000000000000000000, -1.000000000000000000, 0.000000000000000000 ) ) ;
#4913 = CYLINDRICAL_SURFACE ( 'NONE', #3768, 3.000000000000002665 ) ;
#4914 = ORIENTED_EDGE ( 'NONE', *, *, #18272, .F. ) ;
#4915 = CARTESIAN_POINT ( 'NONE',  ( -5.345822467930000599, 40.94956462150000220, -144.4907973060000188 ) ) ;
#4916 = DIRECTION ( 'NONE',  ( 1.000000000000000000, 0.000000000000000000, -1.701177084980000217E-20 ) ) ;
#4917 = CARTESIAN_POINT ( 'NONE',  ( -9.292483939661099868, 40.96918990792104154, -144.3907905727577941 ) ) ;
#4918 = DIRECTION ( 'NONE',  ( 1.000000000000000000, 0.000000000000000000, 0.000000000000000000 ) ) ;
#4919 = VERTEX_POINT ( 'NONE', #22719 ) ;
#4920 = CIRCLE ( 'NONE', #15939, 0.5000000000000004441 ) ;
#4921 =( NAMED_UNIT ( * ) PLANE_ANGLE_UNIT ( ) SI_UNIT ( $, .RADIAN. ) );
#4922 = EDGE_CURVE ( 'NONE', #9664, #1217, #6414, .T. ) ;
#4923 = VECTOR ( 'NONE', #1793, 1000.000000000000000 ) ;
#4924 = EDGE_CURVE ( 'NONE', #1380, #12665, #21659, .T. ) ;
#4925 = ORIENTED_EDGE ( 'NONE', *, *, #18827, .F. ) ;
#4926 = CARTESIAN_POINT ( 'NONE',  ( -7.812322887936786309, 34.92289332027021231, -141.3159265060239704 ) ) ;
#4927 = CARTESIAN_POINT ( 'NONE',  ( -32.50000000000000000, -50.50000000000000000, -149.5552959529999839 ) ) ;
#4928 = DIRECTION ( 'NONE',  ( -4.510170015240000199E-12, 1.314504061159999897E-13, -1.000000000000000000 ) ) ;
#4929 = CIRCLE ( 'NONE', #378, 1.499999999999999556 ) ;
#4930 = EDGE_LOOP ( 'NONE', ( #12417, #18754, #11793 ) ) ;
#4931 = VECTOR ( 'NONE', #23024, 1000.000000000000000 ) ;
#4932 = CARTESIAN_POINT ( 'NONE',  ( -35.07300000000000040, 14.00000000000000000, -143.5552959529999839 ) ) ;
#4933 = CARTESIAN_POINT ( 'NONE',  ( 2.218297500549999857, -15.44723318490000175, -147.5552959529999839 ) ) ;
#4934 = EDGE_LOOP ( 'NONE', ( #13852, #23056, #12106, #20693, #9620 ) ) ;
#4935 = CARTESIAN_POINT ( 'NONE',  ( -21.89685178203216864, 37.04474463553891184, -147.4979728337013682 ) ) ;
#4936 = CARTESIAN_POINT ( 'NONE',  ( -18.18930989797999942, 36.96028804431571757, -147.6841622079159890 ) ) ;
#4937 = FACE_OUTER_BOUND ( 'NONE', #9115, .T. ) ;
#4938 = CARTESIAN_POINT ( 'NONE',  ( -13.86630785130000021, 51.50000000000000000, -137.0552959530000123 ) ) ;
#4939 = CARTESIAN_POINT ( 'NONE',  ( -7.010349701930000066, 37.05829245179999987, -148.1453878979999956 ) ) ;
#4940 = CARTESIAN_POINT ( 'NONE',  ( -15.68268784160000173, 36.02211616019999951, -148.5535485649999998 ) ) ;
#4941 = CARTESIAN_POINT ( 'NONE',  ( 18.95053822279999878, -50.00000000000000000, -149.5552959529999839 ) ) ;
#4942 = CIRCLE ( 'NONE', #18630, 0.7500000000000006661 ) ;
#4943 = LINE ( 'NONE', #10504, #5938 ) ;
#4944 = AXIS2_PLACEMENT_3D ( 'NONE', #2913, #13607, #10144 ) ;
#4945 = CIRCLE ( 'NONE', #18252, 2.000000000000001776 ) ;
#4946 = AXIS2_PLACEMENT_3D ( 'NONE', #6533, #13802, #3560 ) ;
#4947 = VERTEX_POINT ( 'NONE', #122 ) ;
#4948 = DIRECTION ( 'NONE',  ( 1.000000000000000000, 0.000000000000000000, -8.955799065309598247E-12 ) ) ;
#4949 = PRODUCT_DEFINITION_CONTEXT ( 'detailed design', #9462, 'design' ) ;
#4950 = EDGE_CURVE ( 'NONE', #10763, #5071, #22748, .T. ) ;
#4951 = ORIENTED_EDGE ( 'NONE', *, *, #6206, .F. ) ;
#4952 = EDGE_CURVE ( 'NONE', #4709, #22352, #16057, .T. ) ;
#4953 = ORIENTED_EDGE ( 'NONE', *, *, #20582, .T. ) ;
#4954 = FACE_OUTER_BOUND ( 'NONE', #1545, .T. ) ;
#4955 = CARTESIAN_POINT ( 'NONE',  ( -28.18916860660990764, 34.88657501822456908, -140.9963367595939872 ) ) ;
#4956 = EDGE_CURVE ( 'NONE', #4286, #21227, #10911, .T. ) ;
#4957 = ORIENTED_EDGE ( 'NONE', *, *, #19000, .F. ) ;
#4958 = ORIENTED_EDGE ( 'NONE', *, *, #19703, .F. ) ;
#4959 = CARTESIAN_POINT ( 'NONE',  ( -15.00000000000000000, -43.00000000000000000, -145.5552959529999839 ) ) ;
#4960 = CARTESIAN_POINT ( 'NONE',  ( 10.68320006080000084, -21.50000000000000000, -138.5552959529999839 ) ) ;
#4961 = CARTESIAN_POINT ( 'NONE',  ( -12.30631862551127931, 40.23402543387735619, -145.9987124283914000 ) ) ;
#4962 = FACE_OUTER_BOUND ( 'NONE', #14163, .T. ) ;
#4963 = VECTOR ( 'NONE', #6909, 1000.000000000000000 ) ;
#4964 = VECTOR ( 'NONE', #8838, 1000.000000000000000 ) ;
#4965 = DIRECTION ( 'NONE',  ( 1.527666881879999979E-13, 8.100187187669999987E-13, 1.000000000000000000 ) ) ;
#4966 = VERTEX_POINT ( 'NONE', #10557 ) ;
#4967 = CARTESIAN_POINT ( 'NONE',  ( -28.90798551740000022, 37.01360947639999921, -139.5686590450000040 ) ) ;
#4968 = CARTESIAN_POINT ( 'NONE',  ( 6.000000000010000001, -3.500000000000000000, -136.0552959530000123 ) ) ;
#4969 = CARTESIAN_POINT ( 'NONE',  ( -17.23482902069999767, -18.00000000000000000, -144.8157682190000060 ) ) ;
#4970 = ORIENTED_EDGE ( 'NONE', *, *, #19000, .T. ) ;
#4971 = PLANE ( 'NONE',  #60 ) ;
#4972 = ORIENTED_EDGE ( 'NONE', *, *, #9302, .T. ) ;
#4973 = CARTESIAN_POINT ( 'NONE',  ( -20.74418227179999974, 39.28578094470000082, -147.3492911870000057 ) ) ;
#4974 = CARTESIAN_POINT ( 'NONE',  ( 0.5000000001340000333, 24.10555127549999810, -150.5552959529999839 ) ) ;
#4975 = ORIENTED_EDGE ( 'NONE', *, *, #3419, .T. ) ;
#4976 = PLANE ( 'NONE',  #13287 ) ;
#4977 = FACE_OUTER_BOUND ( 'NONE', #21229, .T. ) ;
#4978 = EDGE_LOOP ( 'NONE', ( #2501, #16403, #19719, #4427, #14728 ) ) ;
#4979 = EDGE_CURVE ( 'NONE', #20921, #10191, #16029, .T. ) ;
#4980 = CARTESIAN_POINT ( 'NONE',  ( -15.03885004549999849, 41.12207116019999376, -146.4108951270000034 ) ) ;
#4981 = CARTESIAN_POINT ( 'NONE',  ( -24.94748837732958080, 34.18267032390015459, -147.9795192610947367 ) ) ;
#4982 = EDGE_CURVE ( 'NONE', #5391, #576, #3444, .T. ) ;
#4983 = VERTEX_POINT ( 'NONE', #5573 ) ;
#4984 = PRESENTATION_STYLE_ASSIGNMENT (( #19966 ) ) ;
#4985 = ORIENTED_EDGE ( 'NONE', *, *, #8504, .F. ) ;
#4986 = CARTESIAN_POINT ( 'NONE',  ( -6.601136089949999786, -20.10368962670000315, -144.5552959529999839 ) ) ;
#4987 = LINE ( 'NONE', #22962, #15681 ) ;
#4988 = ORIENTED_EDGE ( 'NONE', *, *, #21807, .T. ) ;
#4989 = FACE_OUTER_BOUND ( 'NONE', #5572, .T. ) ;
#4990 = PRODUCT_DEFINITION ( 'UNKNOWN', '', #4686, #23270 ) ;
#4991 = LINE ( 'NONE', #8651, #13628 ) ;
#4992 = EDGE_CURVE ( 'NONE', #23292, #3037, #19868, .T. ) ;
#4993 = CARTESIAN_POINT ( 'NONE',  ( 4.500000000000000000, -3.500000000000000000, -145.5552959529999839 ) ) ;
#4994 = VECTOR ( 'NONE', #4800, 1000.000000000000000 ) ;
#4995 = CIRCLE ( 'NONE', #8012, 0.5000000000000009992 ) ;
#4996 = ORIENTED_EDGE ( 'NONE', *, *, #9777, .T. ) ;
#4997 = DIRECTION ( 'NONE',  ( 0.000000000000000000, -2.956752937091289955E-12, -1.000000000000000000 ) ) ;
#4998 = EDGE_CURVE ( 'NONE', #10751, #18293, #18314, .T. ) ;
#4999 = DIRECTION ( 'NONE',  ( -1.000000000000000000, 0.000000000000000000, 0.000000000000000000 ) ) ;
#5000 = CARTESIAN_POINT ( 'NONE',  ( -14.40511015815818041, 39.11695720675039212, -141.1121292871179946 ) ) ;
#5001 = CARTESIAN_POINT ( 'NONE',  ( -29.18503926097451995, 39.40432144733799902, -139.9690405635991794 ) ) ;
#5002 = ORIENTED_EDGE ( 'NONE', *, *, #14270, .F. ) ;
#5003 = CARTESIAN_POINT ( 'NONE',  ( -15.19923223292398795, -41.50000000000003553, -136.0552959529657073 ) ) ;
#5004 = CARTESIAN_POINT ( 'NONE',  ( -2.499999999940000439, 37.00000000000000000, -144.0552959529999839 ) ) ;
#5005 = CARTESIAN_POINT ( 'NONE',  ( 26.50000000000000000, -20.10730091830127009, -150.0552959530000123 ) ) ;
#5006 = DIRECTION ( 'NONE',  ( 1.000000000000000000, 0.000000000000000000, 0.000000000000000000 ) ) ;
#5007 = LINE ( 'NONE', #14528, #21361 ) ;
#5008 = LINE ( 'NONE', #3223, #11331 ) ;
#5009 = VECTOR ( 'NONE', #1574, 1000.000000000000000 ) ;
#5010 = EDGE_CURVE ( 'NONE', #3075, #8221, #18193, .T. ) ;
#5011 = ORIENTED_EDGE ( 'NONE', *, *, #2885, .T. ) ;
#5012 = AXIS2_PLACEMENT_3D ( 'NONE', #5622, #8214, #17388 ) ;
#5013 = VECTOR ( 'NONE', #23099, 1000.000000000000114 ) ;
#5014 = CARTESIAN_POINT ( 'NONE',  ( -4.499999999959999109, 40.00000000000000000, -136.0552959530000123 ) ) ;
#5015 = DIRECTION ( 'NONE',  ( 1.000000000000000000, 0.000000000000000000, 0.000000000000000000 ) ) ;
#5016 = PLANE ( 'NONE',  #22887 ) ;
#5017 = LINE ( 'NONE', #16620, #22507 ) ;
#5018 = DIRECTION ( 'NONE',  ( -1.000000000000000000, -3.994014902950000436E-29, 0.000000000000000000 ) ) ;
#5019 = ORIENTED_EDGE ( 'NONE', *, *, #13843, .T. ) ;
#5020 = FACE_OUTER_BOUND ( 'NONE', #4644, .T. ) ;
#5021 = EDGE_CURVE ( 'NONE', #20985, #13908, #2204, .T. ) ;
#5022 = CARTESIAN_POINT ( 'NONE',  ( -26.29566636579999894, 36.18167175180000328, -140.3932108110000172 ) ) ;
#5023 = ORIENTED_EDGE ( 'NONE', *, *, #679, .F. ) ;
#5024 = CARTESIAN_POINT ( 'NONE',  ( -32.50000000000000000, 14.00000000000000000, -144.0552959529999839 ) ) ;
#5025 = AXIS2_PLACEMENT_3D ( 'NONE', #4590, #17084, #1161 ) ;
#5026 = CYLINDRICAL_SURFACE ( 'NONE', #22767, 1.500000000000001332 ) ;
#5027 = ORIENTED_EDGE ( 'NONE', *, *, #23478, .F. ) ;
#5028 = AXIS2_PLACEMENT_3D ( 'NONE', #20089, #7692, #9245 ) ;
#5029 = CARTESIAN_POINT ( 'NONE',  ( -34.50000000000000000, -74.00000000000000000, -144.0552959529999839 ) ) ;
#5030 = EDGE_CURVE ( 'NONE', #7233, #3293, #12708, .T. ) ;
#5031 = DIRECTION ( 'NONE',  ( 0.000000000000000000, -1.000000000000000000, 0.000000000000000000 ) ) ;
#5032 = EDGE_CURVE ( 'NONE', #17345, #12862, #21419, .T. ) ;
#5033 = DIRECTION ( 'NONE',  ( 0.000000000000000000, -1.000000000000000000, 0.000000000000000000 ) ) ;
#5034 = CARTESIAN_POINT ( 'NONE',  ( 7.136768929676958528, 37.62588656037802082, -141.6348998444176743 ) ) ;
#5035 = ORIENTED_EDGE ( 'NONE', *, *, #13018, .F. ) ;
#5036 = CARTESIAN_POINT ( 'NONE',  ( -10.24572398529664063, 36.15958899794869552, -148.2198882318936910 ) ) ;
#5037 = CARTESIAN_POINT ( 'NONE',  ( -0.6175362654710214727, 22.91577772018773729, -150.0552959529999839 ) ) ;
#5038 = EDGE_CURVE ( 'NONE', #6002, #22754, #8383, .T. ) ;
#5039 = FACE_OUTER_BOUND ( 'NONE', #6999, .T. ) ;
#5040 = CARTESIAN_POINT ( 'NONE',  ( 3.839256068031374536, -32.96302158184152375, -136.0552959530086525 ) ) ;
#5041 = EDGE_CURVE ( 'NONE', #21465, #8058, #461, .T. ) ;
#5042 = VERTEX_POINT ( 'NONE', #17102 ) ;
#5043 = PRESENTATION_STYLE_ASSIGNMENT (( #12283 ) ) ;
#5044 = ORIENTED_EDGE ( 'NONE', *, *, #1826, .F. ) ;
#5045 = CARTESIAN_POINT ( 'NONE',  ( -6.812760379890000273, 32.88798608609999974, -143.6676051400000063 ) ) ;
#5046 = CARTESIAN_POINT ( 'NONE',  ( -6.807579269459999693, 38.78453684440000160, -147.8970667739999953 ) ) ;
#5047 =( GEOMETRIC_REPRESENTATION_CONTEXT ( 3 ) GLOBAL_UNCERTAINTY_ASSIGNED_CONTEXT ( ( #1631 ) ) GLOBAL_UNIT_ASSIGNED_CONTEXT ( ( #2207, #22188, #9311 ) ) REPRESENTATION_CONTEXT ( 'NONE', 'WORKASPACE' ) );
#5048 = CARTESIAN_POINT ( 'NONE',  ( 25.50000000000000000, 22.50000000000000000, -150.0552959529999839 ) ) ;
#5049 = AXIS2_PLACEMENT_3D ( 'NONE', #12374, #6563, #17743 ) ;
#5050 = VERTEX_POINT ( 'NONE', #11606 ) ;
#5051 = CARTESIAN_POINT ( 'NONE',  ( -9.347107914279998653, -17.32706600430000066, -144.5552959529999839 ) ) ;
#5052 = DIRECTION ( 'NONE',  ( 0.000000000000000000, -1.000000000000000000, 8.159623473500000156E-13 ) ) ;
#5053 = ORIENTED_EDGE ( 'NONE', *, *, #19842, .T. ) ;
#5054 = PLANE ( 'NONE',  #8381 ) ;
#5055 = EDGE_CURVE ( 'NONE', #1186, #10902, #22461, .T. ) ;
#5056 = DIRECTION ( 'NONE',  ( 0.000000000000000000, 0.000000000000000000, 1.000000000000000000 ) ) ;
#5057 = CARTESIAN_POINT ( 'NONE',  ( -17.39900052719454138, -41.15635984007523973, -150.0552959530000123 ) ) ;
#5058 = CARTESIAN_POINT ( 'NONE',  ( 4.750000000030000002, -44.75000000000000000, -136.0552959530000123 ) ) ;
#5059 = CYLINDRICAL_SURFACE ( 'NONE', #23406, 2.000000000000001776 ) ;
#5060 = EDGE_CURVE ( 'NONE', #1276, #8640, #22011, .T. ) ;
#5061 = DIRECTION ( 'NONE',  ( 2.507554887169999917E-12, 0.000000000000000000, -1.000000000000000000 ) ) ;
#5062 = LINE ( 'NONE', #12306, #11250 ) ;
#5063 = COLOUR_RGB ( '', 0.31764706, 0.68627451, 0.89019608) ;
#5064 = DIRECTION ( 'NONE',  ( 0.000000000000000000, -1.000000000000000000, 3.568879590630000244E-13 ) ) ;
#5065 = ORIENTED_EDGE ( 'NONE', *, *, #15126, .F. ) ;
#5066 = DIRECTION ( 'NONE',  ( 8.955190032050000935E-12, -9.104778821549999739E-13, 1.000000000000000000 ) ) ;
#5067 = EDGE_LOOP ( 'NONE', ( #7161, #6503, #20402, #13366 ) ) ;
#5068 = ORIENTED_EDGE ( 'NONE', *, *, #14997, .T. ) ;
#5069 = CARTESIAN_POINT ( 'NONE',  ( -34.50000000000000000, 46.00000000000000000, -141.5552959529999839 ) ) ;
#5070 = CARTESIAN_POINT ( 'NONE',  ( 6.500000000159999125, 20.50000000000000000, -139.5552959529999839 ) ) ;
#5071 = VERTEX_POINT ( 'NONE', #4259 ) ;
#5072 = EDGE_LOOP ( 'NONE', ( #12436, #19935, #10941, #11211 ) ) ;
#5073 = CARTESIAN_POINT ( 'NONE',  ( -5.985028652404004390, 19.88109793996616403, -150.0552959529999839 ) ) ;
#5074 = CARTESIAN_POINT ( 'NONE',  ( -19.48816230409999761, 36.23023348070000083, -140.2952556289999961 ) ) ;
#5075 = CARTESIAN_POINT ( 'NONE',  ( -12.57385931496360065, 38.47543513205931731, -147.4253642442816101 ) ) ;
#5076 = DIRECTION ( 'NONE',  ( 0.000000000000000000, 0.000000000000000000, -1.000000000000000000 ) ) ;
#5077 = CARTESIAN_POINT ( 'NONE',  ( -7.753123200440416696, 36.02113668015080350, -139.3990843276119449 ) ) ;
#5078 = ORIENTED_EDGE ( 'NONE', *, *, #19723, .T. ) ;
#5079 = CARTESIAN_POINT ( 'NONE',  ( 9.346855175913132641, 35.76186543769073012, -141.8834125995852844 ) ) ;
#5080 = EDGE_CURVE ( 'NONE', #4452, #947, #21998, .T. ) ;
#5081 = CARTESIAN_POINT ( 'NONE',  ( -8.514310886080000529, 36.94123471670000214, -140.1199228270000106 ) ) ;
#5082 = DIRECTION ( 'NONE',  ( -2.507771768019999718E-12, -1.592654864069999939E-17, 1.000000000000000000 ) ) ;
#5083 = ORIENTED_EDGE ( 'NONE', *, *, #7538, .F. ) ;
#5084 = CARTESIAN_POINT ( 'NONE',  ( -21.35824191589185972, -4.000000000000000000, -149.4708568729758724 ) ) ;
#5085 = ORIENTED_EDGE ( 'NONE', *, *, #21376, .T. ) ;
#5086 = DIRECTION ( 'NONE',  ( 1.000000000000000000, 0.000000000000000000, -2.257171095940000041E-12 ) ) ;
#5087 = CARTESIAN_POINT ( 'NONE',  ( -14.47770030809999930, -34.50000000000000000, -149.3052959529999839 ) ) ;
#5088 = EDGE_LOOP ( 'NONE', ( #7, #16480, #19975, #17867 ) ) ;
#5089 = CARTESIAN_POINT ( 'NONE',  ( 4.999999999879999990, -3.000000000000000000, -135.0552959530000123 ) ) ;
#5090 = CARTESIAN_POINT ( 'NONE',  ( 19.68320006079999729, -20.50000000000000000, -148.5552959529999839 ) ) ;
#5091 = ORIENTED_EDGE ( 'NONE', *, *, #19999, .T. ) ;
#5092 = VECTOR ( 'NONE', #5623, 1000.000000000000000 ) ;
#5093 = CARTESIAN_POINT ( 'NONE',  ( -21.63220705382456899, 37.01315499804844222, -148.7192284428847415 ) ) ;
#5094 = FACE_OUTER_BOUND ( 'NONE', #18289, .T. ) ;
#5095 = ORIENTED_EDGE ( 'NONE', *, *, #9122, .F. ) ;
#5096 = EDGE_LOOP ( 'NONE', ( #11711, #1816, #10133, #16959, #23288 ) ) ;
#5097 = LINE ( 'NONE', #14614, #15947 ) ;
#5098 = CARTESIAN_POINT ( 'NONE',  ( 0.000000000000000000, 0.000000000000000000, -140.0552959529999839 ) ) ;
#5099 = VERTEX_POINT ( 'NONE', #339 ) ;
#5100 = LINE ( 'NONE', #14264, #12152 ) ;
#5101 = CARTESIAN_POINT ( 'NONE',  ( -25.86630785129999666, -51.00000000000000000, -137.0552959530000123 ) ) ;
#5102 = ORIENTED_EDGE ( 'NONE', *, *, #6464, .F. ) ;
#5103 = CARTESIAN_POINT ( 'NONE',  ( -16.81794493339999619, 37.02435727940000731, -140.5111119820000170 ) ) ;
#5104 = ADVANCED_FACE ( 'NONE', ( #18771 ), #12942, .F. ) ;
#5105 = VECTOR ( 'NONE', #8484, 1000.000000000000000 ) ;
#5106 = ADVANCED_FACE ( 'NONE', ( #15207 ), #20443, .F. ) ;
#5107 = VERTEX_POINT ( 'NONE', #22340 ) ;
#5108 = DIRECTION ( 'NONE',  ( 1.000000000000000000, 2.688820921349999492E-17, 0.000000000000000000 ) ) ;
#5109 = CARTESIAN_POINT ( 'NONE',  ( -0.7500000000009999779, -50.00000000000000000, -149.5552959529999839 ) ) ;
#5110 = CARTESIAN_POINT ( 'NONE',  ( -15.24898703717404125, 36.96741147809888162, -148.5896301378343196 ) ) ;
#5111 = CARTESIAN_POINT ( 'NONE',  ( 0.5000000001659999915, 16.89444872450000190, -136.5552959530000123 ) ) ;
#5112 = ORIENTED_EDGE ( 'NONE', *, *, #2755, .F. ) ;
#5113 = SURFACE_SIDE_STYLE ('',( #8904 ) ) ;
#5114 = LINE ( 'NONE', #10565, #11202 ) ;
#5115 = FACE_OUTER_BOUND ( 'NONE', #19090, .T. ) ;
#5116 = LINE ( 'NONE', #12252, #16706 ) ;
#5117 = DIRECTION ( 'NONE',  ( 1.000000000000000000, 0.000000000000000000, 2.504935852220000146E-12 ) ) ;
#5118 = LINE ( 'NONE', #23212, #1113 ) ;
#5119 = VERTEX_POINT ( 'NONE', #22228 ) ;
#5120 = CARTESIAN_POINT ( 'NONE',  ( 32.00000000000000000, -33.03620104880000241, -137.0552959530000123 ) ) ;
#5121 = DIRECTION ( 'NONE',  ( 9.087266560786239640E-12, 0.000000000000000000, 1.000000000000000000 ) ) ;
#5122 = PLANE ( 'NONE',  #17434 ) ;
#5123 = CARTESIAN_POINT ( 'NONE',  ( -5.765044504979666584, 41.82099204264250858, -144.5279374446441238 ) ) ;
#5124 = CARTESIAN_POINT ( 'NONE',  ( -32.50000000000000000, -50.50000000000000000, -137.0552959530000123 ) ) ;
#5125 = CARTESIAN_POINT ( 'NONE',  ( -6.774730888589999722, 50.00000000000000000, -151.0552959529999839 ) ) ;
#5126 = ORIENTED_EDGE ( 'NONE', *, *, #8066, .F. ) ;
#5127 = LINE ( 'NONE', #4782, #6943 ) ;
#5128 = CARTESIAN_POINT ( 'NONE',  ( 5.809692093864619267, -2.742832019563268720, -150.0552959530000123 ) ) ;
#5129 = ORIENTED_EDGE ( 'NONE', *, *, #14500, .T. ) ;
#5130 = LINE ( 'NONE', #19656, #6815 ) ;
#5131 = ORIENTED_EDGE ( 'NONE', *, *, #17779, .F. ) ;
#5132 = CARTESIAN_POINT ( 'NONE',  ( -24.84704225922425280, 37.03879906167826164, -147.5513581852341360 ) ) ;
#5133 = PLANE ( 'NONE',  #7444 ) ;
#5134 = DIRECTION ( 'NONE',  ( 1.000000000000000000, 0.000000000000000000, -2.253752739989067373E-12 ) ) ;
#5135 = CARTESIAN_POINT ( 'NONE',  ( 7.255075146305371980, 36.16322928933654168, -141.6994869973446498 ) ) ;
#5136 = VECTOR ( 'NONE', #2668, 1000.000000000000000 ) ;
#5137 = ORIENTED_EDGE ( 'NONE', *, *, #9808, .F. ) ;
#5138 =( NAMED_UNIT ( * ) PLANE_ANGLE_UNIT ( ) SI_UNIT ( $, .RADIAN. ) );
#5139 = FACE_OUTER_BOUND ( 'NONE', #5145, .T. ) ;
#5140 = CARTESIAN_POINT ( 'NONE',  ( 13.13369214859999978, 51.00000000000000000, -137.0552959530000123 ) ) ;
#5141 = DIRECTION ( 'NONE',  ( -1.000000000000000000, 0.000000000000000000, 0.000000000000000000 ) ) ;
#5142 = EDGE_CURVE ( 'NONE', #7247, #6997, #6156, .T. ) ;
#5143 = ORIENTED_EDGE ( 'NONE', *, *, #3389, .T. ) ;
#5144 = DIRECTION ( 'NONE',  ( 0.000000000000000000, 1.000000000000000000, 0.000000000000000000 ) ) ;
#5145 = EDGE_LOOP ( 'NONE', ( #8880, #15457, #5544, #4985 ) ) ;
#5146 = CARTESIAN_POINT ( 'NONE',  ( -7.484002448341838587, 33.56044099697500371, -143.7975408956788215 ) ) ;
#5147 = CARTESIAN_POINT ( 'NONE',  ( -23.03778781510000329, 40.78628791080000582, -141.9896475660000306 ) ) ;
#5148 = CARTESIAN_POINT ( 'NONE',  ( 23.89222110089999873, -31.59487100459999809, -145.5552959529999839 ) ) ;
#5149 = EDGE_CURVE ( 'NONE', #23117, #22098, #14967, .T. ) ;
#5150 = ORIENTED_EDGE ( 'NONE', *, *, #23485, .F. ) ;
#5151 = DIRECTION ( 'NONE',  ( 2.257171095940000041E-12, 1.003664318209372040E-28, 1.000000000000000000 ) ) ;
#5152 = DIRECTION ( 'NONE',  ( 8.956391184260000029E-12, -9.112710586119999183E-13, 1.000000000000000000 ) ) ;
#5153 = EDGE_CURVE ( 'NONE', #3899, #19799, #15081, .T. ) ;
#5154 = AXIS2_PLACEMENT_3D ( 'NONE', #1090, #13815, #21079 ) ;
#5155 = ORIENTED_EDGE ( 'NONE', *, *, #13911, .T. ) ;
#5156 = CARTESIAN_POINT ( 'NONE',  ( -17.98964812810000069, 38.50830570029999933, -147.4920370689999913 ) ) ;
#5157 = ADVANCED_FACE ( 'NONE', ( #13291 ), #4138, .T. ) ;
#5158 = EDGE_CURVE ( 'NONE', #954, #10456, #9823, .T. ) ;
#5159 = PLANE ( 'NONE',  #10966 ) ;
#5160 = CARTESIAN_POINT ( 'NONE',  ( -12.00000000000000000, -42.60730091830127719, -150.0552959530000123 ) ) ;
#5161 = CARTESIAN_POINT ( 'NONE',  ( 8.750000000029995562, -45.01504245778616564, -136.0552959530197654 ) ) ;
#5162 = CARTESIAN_POINT ( 'NONE',  ( 19.45666326950000169, 50.88169314249999786, -150.0552959529999839 ) ) ;
#5163 = CARTESIAN_POINT ( 'NONE',  ( -15.79202522179999946, 35.03772048769999969, -148.2850092029999871 ) ) ;
#5164 = CARTESIAN_POINT ( 'NONE',  ( -33.50000000000000000, -35.00000000000000000, -140.0552959529999839 ) ) ;
#5165 = CARTESIAN_POINT ( 'NONE',  ( -35.07300000000000040, 16.55147016440000129, -144.5552959529999839 ) ) ;
#5166 = CARTESIAN_POINT ( 'NONE',  ( 32.05742780150000470, 40.87448416799999507, -149.5552959529999839 ) ) ;
#5167 = VERTEX_POINT ( 'NONE', #3917 ) ;
#5168 = VECTOR ( 'NONE', #2190, 1000.000000000000000 ) ;
#5169 = CARTESIAN_POINT ( 'NONE',  ( 6.500000000140000012, 20.50000000000000000, -147.5552959529999839 ) ) ;
#5170 = AXIS2_PLACEMENT_3D ( 'NONE', #1349, #1120, #15847 ) ;
#5171 = UNCERTAINTY_MEASURE_WITH_UNIT (LENGTH_MEASURE( 1.000000000000000082E-05 ), #18238, 'distance_accuracy_value', 'NONE');
#5172 = ORIENTED_EDGE ( 'NONE', *, *, #7232, .F. ) ;
#5173 = B_SPLINE_CURVE_WITH_KNOTS ( 'NONE', 5,
 ( #11814, #2683, #3039, #19200, #15400, #22659, #19092, #10276, #10025, #17301, #15517, #22779 ),
 .UNSPECIFIED., .F., .F.,
 ( 6, 3, 3, 6 ),
 ( 0.000000000000000000, 4.151671928079999851, 8.316542232069998875, 12.50501063799999990 ),
 .UNSPECIFIED. ) ;
#5174 = ORIENTED_EDGE ( 'NONE', *, *, #5620, .F. ) ;
#5175 = DIRECTION ( 'NONE',  ( -1.000000000000000000, 0.000000000000000000, 2.257076750620000196E-12 ) ) ;
#5176 = CARTESIAN_POINT ( 'NONE',  ( -28.19843657148410188, 33.49775354811340122, -143.6175028023312166 ) ) ;
#5177 = ORIENTED_EDGE ( 'NONE', *, *, #20846, .F. ) ;
#5178 = DIRECTION ( 'NONE',  ( 0.000000000000000000, 0.000000000000000000, 1.000000000000000000 ) ) ;
#5179 = ADVANCED_FACE ( 'NONE', ( #5917 ), #18423, .T. ) ;
#5180 = ORIENTED_EDGE ( 'NONE', *, *, #6691, .F. ) ;
#5181 = LINE ( 'NONE', #7090, #10225 ) ;
#5182 = CARTESIAN_POINT ( 'NONE',  ( -19.61368621442406024, 33.72156397702593011, -146.2040437318905788 ) ) ;
#5183 = EDGE_CURVE ( 'NONE', #12670, #11634, #14857, .T. ) ;
#5184 = CARTESIAN_POINT ( 'NONE',  ( -11.09715128152969754, 40.92510525134454014, -143.8328159740042338 ) ) ;
#5185 = CARTESIAN_POINT ( 'NONE',  ( -13.86630785130000021, -51.50000000000000000, -136.0552959530000123 ) ) ;
#5186 = ORIENTED_EDGE ( 'NONE', *, *, #8212, .F. ) ;
#5187 = LINE ( 'NONE', #5545, #21691 ) ;
#5188 = EDGE_CURVE ( 'NONE', #21084, #4592, #1879, .T. ) ;
#5189 = ORIENTED_EDGE ( 'NONE', *, *, #22222, .T. ) ;
#5190 = CARTESIAN_POINT ( 'NONE',  ( 9.999995540850324716, 36.80846206152234856, -141.5553035006076072 ) ) ;
#5191 = VECTOR ( 'NONE', #5198, 1000.000000000000000 ) ;
#5192 = DIRECTION ( 'NONE',  ( -4.430233957459999899E-12, 6.110667527539999876E-13, -1.000000000000000000 ) ) ;
#5193 = LINE ( 'NONE', #5440, #21662 ) ;
#5194 = ORIENTED_EDGE ( 'NONE', *, *, #12324, .F. ) ;
#5195 = CARTESIAN_POINT ( 'NONE',  ( 3.000000000010000001, -3.500000000000000000, -136.5552959530000123 ) ) ;
#5196 = VERTEX_POINT ( 'NONE', #11257 ) ;
#5197 = DIRECTION ( 'NONE',  ( -1.000000000000000000, -2.602084704489999637E-17, 2.257171095940000041E-12 ) ) ;
#5198 = DIRECTION ( 'NONE',  ( 0.000000000000000000, -2.256683728769999802E-12, 1.000000000000000000 ) ) ;
#5200 = VERTEX_POINT ( 'NONE', #2249 ) ;
#5199 = AXIS2_PLACEMENT_3D ( 'NONE', #18505, #4108, #22314 ) ;
#5201 = CARTESIAN_POINT ( 'NONE',  ( -12.08222824379999949, 38.77433534089999512, -148.2726881729999775 ) ) ;
#5202 = VERTEX_POINT ( 'NONE', #17332 ) ;
#5203 = CARTESIAN_POINT ( 'NONE',  ( -22.52056272209999932, 33.27763168300000274, -146.2006519230000094 ) ) ;
#5204 = AXIS2_PLACEMENT_3D ( 'NONE', #7588, #14627, #15408 ) ;
#5205 = DIRECTION ( 'NONE',  ( 2.255973186040000320E-12, 0.000000000000000000, 1.000000000000000000 ) ) ;
#5206 = EDGE_LOOP ( 'NONE', ( #11620, #3532, #11456, #23131, #12096 ) ) ;
#5207 = ADVANCED_FACE ( 'NONE', ( #8044 ), #10180, .T. ) ;
#5208 = ORIENTED_EDGE ( 'NONE', *, *, #11081, .T. ) ;
#5209 = PRODUCT ( 'Phillips Screw', 'Phillips Screw', '', ( #18304 ) ) ;
#5210 = CARTESIAN_POINT ( 'NONE',  ( -0.7499999998590000105, 41.50000000000000000, -147.5552959529999839 ) ) ;
#5211 = EDGE_CURVE ( 'NONE', #4474, #6561, #3869, .T. ) ;
#5212 = CARTESIAN_POINT ( 'NONE',  ( -11.38486064709999823, 36.95668670079999885, -140.3965526140000009 ) ) ;
#5213 = ORIENTED_EDGE ( 'NONE', *, *, #19694, .T. ) ;
#5214 = DIRECTION ( 'NONE',  ( 2.839308199620000013E-14, 3.568879590630000244E-13, 1.000000000000000000 ) ) ;
#5215 = DIRECTION ( 'NONE',  ( -0.09503188512734457583, -0.9954742291034677226, 2.970706163671393545E-13 ) ) ;
#5216 = PLANE ( 'NONE',  #10958 ) ;
#5217 = ORIENTED_EDGE ( 'NONE', *, *, #1007, .F. ) ;
#5218 = CARTESIAN_POINT ( 'NONE',  ( -2.273230205684010574, 46.10147512692400085, -150.0552959530000123 ) ) ;
#5219 = VECTOR ( 'NONE', #3601, 1000.000000000000000 ) ;
#5220 = VECTOR ( 'NONE', #642, 1000.000000000000114 ) ;
#5221 = ORIENTED_EDGE ( 'NONE', *, *, #18484, .T. ) ;
#5222 = DIRECTION ( 'NONE',  ( 0.000000000000000000, 4.009147065150000317E-51, -1.000000000000000000 ) ) ;
#5223 = CARTESIAN_POINT ( 'NONE',  ( -20.70396626025547349, -4.379374642480768465, -146.3157682190058893 ) ) ;
#5224 = CARTESIAN_POINT ( 'NONE',  ( -15.04288342797402578, 38.87661853468269868, -148.3497549206679480 ) ) ;
#5225 = CARTESIAN_POINT ( 'NONE',  ( -28.46722477587058009, 38.15066728402772611, -140.0554881084096053 ) ) ;
#5226 = VERTEX_POINT ( 'NONE', #8277 ) ;
#5227 = CARTESIAN_POINT ( 'NONE',  ( -0.9999999999639996862, 20.00701398444611101, -136.0552959529977954 ) ) ;
#5228 = LINE ( 'NONE', #14633, #7813 ) ;
#5229 = CARTESIAN_POINT ( 'NONE',  ( -4.946601369560000627, -23.77962690289999870, -144.5552959529999839 ) ) ;
#5230 = CARTESIAN_POINT ( 'NONE',  ( 3.611688725869999975E-11, 42.50000000000000000, -136.0552959530000123 ) ) ;
#5231 = CARTESIAN_POINT ( 'NONE',  ( 12.82492181439999968, -17.92284828160000032, -145.5552959529999839 ) ) ;
#5232 = DIRECTION ( 'NONE',  ( 5.094701932209999624E-24, 1.000000000000000000, -1.149947916579999802E-35 ) ) ;
#5233 = ORIENTED_EDGE ( 'NONE', *, *, #3206, .F. ) ;
#5234 = CARTESIAN_POINT ( 'NONE',  ( -7.499999999969999109, 42.50000000000000000, -137.0552959530000123 ) ) ;
#5235 = AXIS2_PLACEMENT_3D ( 'NONE', #7193, #17339, #12663 ) ;
#5236 = DIRECTION ( 'NONE',  ( 2.257144641397284947E-12, 2.714724913984255017E-24, 1.000000000000000000 ) ) ;
#5237 = EDGE_CURVE ( 'NONE', #9123, #11298, #21272, .T. ) ;
#5238 = CARTESIAN_POINT ( 'NONE',  ( 6.343640159924754940, -5.899000527194532495, -150.0552959529999839 ) ) ;
#5239 =( GEOMETRIC_REPRESENTATION_CONTEXT ( 3 ) GLOBAL_UNCERTAINTY_ASSIGNED_CONTEXT ( ( #23498 ) ) GLOBAL_UNIT_ASSIGNED_CONTEXT ( ( #19987, #10800, #18085 ) ) REPRESENTATION_CONTEXT ( 'NONE', 'WORKASPACE' ) );
#5240 = CARTESIAN_POINT ( 'NONE',  ( -3.500000000000000000, 44.50000000000000000, -151.0552959529999839 ) ) ;
#5241 = CARTESIAN_POINT ( 'NONE',  ( -24.21201708719999957, 40.99356323119999956, -143.6328343570000072 ) ) ;
#5242 = EDGE_CURVE ( 'NONE', #19082, #14999, #16665, .T. ) ;
#5243 = CYLINDRICAL_SURFACE ( 'NONE', #22405, 1.500000000000003331 ) ;
#5244 = VERTEX_POINT ( 'NONE', #15786 ) ;
#5245 = DIRECTION ( 'NONE',  ( 2.506794771760000178E-12, 0.000000000000000000, -1.000000000000000000 ) ) ;
#5246 = DIRECTION ( 'NONE',  ( 1.526468026909999897E-13, 8.159623473500000156E-13, 1.000000000000000000 ) ) ;
#5247 = EDGE_LOOP ( 'NONE', ( #18873, #12800, #10794, #13305, #9427, #9623, #12391, #264 ) ) ;
#5248 =( BOUNDED_CURVE ( )  B_SPLINE_CURVE ( 5, ( #765, #6108, #2441, #9893, #5983, #9659 ),
 .UNSPECIFIED., .F., .F. ) 
 B_SPLINE_CURVE_WITH_KNOTS ( ( 6, 6 ),
 ( 1.570796326695738099, 3.141592653590000062 ),
 .UNSPECIFIED. ) 
 CURVE ( )  GEOMETRIC_REPRESENTATION_ITEM ( )  RATIONAL_B_SPLINE_CURVE ( ( 0.2500000000000000000, 0.2499999999873616097, 0.2999999999810423756, 0.3999999999747231860, 0.5999999999747231971, 1.000000000000000000 ) ) 
 REPRESENTATION_ITEM ( '' )  );
#5249 = PLANE ( 'NONE',  #10604 ) ;
#5250 = EDGE_LOOP ( 'NONE', ( #22987, #11568 ) ) ;
#5251 = DIRECTION ( 'NONE',  ( 1.000000000000000000, 0.000000000000000000, 0.000000000000000000 ) ) ;
#5252 = AXIS2_PLACEMENT_3D ( 'NONE', #8436, #3209, #10441 ) ;
#5253 = CARTESIAN_POINT ( 'NONE',  ( -29.18503926082679811, 39.40432144733731690, -139.9690405636331718 ) ) ;
#5254 = VECTOR ( 'NONE', #11829, 1000.000000000000000 ) ;
#5255 = CARTESIAN_POINT ( 'NONE',  ( 8.500000000050000892, 37.00000000000000000, -149.5552959529999839 ) ) ;
#5256 = CARTESIAN_POINT ( 'NONE',  ( 7.167702963139642058, 37.68962278446276315, -141.6522196278403669 ) ) ;
#5257 = ORIENTED_EDGE ( 'NONE', *, *, #16090, .T. ) ;
#5258 = CARTESIAN_POINT ( 'NONE',  ( -11.29029698159100015, 36.23043332057599741, -140.4049246349841837 ) ) ;
#5259 = CARTESIAN_POINT ( 'NONE',  ( -0.9519686233540903819, 21.48063989304597499, -150.0552959530000123 ) ) ;
#5260 = CARTESIAN_POINT ( 'NONE',  ( -9.515077267811255624, 39.13325659334626039, -146.8938814410688849 ) ) ;
#5261 = CARTESIAN_POINT ( 'NONE',  ( 8.701166446568034729, -31.45126136998390720, -136.0552959530196802 ) ) ;
#5262 = ORIENTED_EDGE ( 'NONE', *, *, #14126, .T. ) ;
#5263 = LINE ( 'NONE', #14665, #3099 ) ;
#5264 = SURFACE_STYLE_USAGE ( .BOTH. , #4803 ) ;
#5265 = ORIENTED_EDGE ( 'NONE', *, *, #3205, .T. ) ;
#5266 = CARTESIAN_POINT ( 'NONE',  ( -17.08727435560000174, -1.500000000000000000, -147.1525923079999814 ) ) ;
#5267 = CARTESIAN_POINT ( 'NONE',  ( -9.282104535860000283, -16.71402168319999859, -145.5552959529999839 ) ) ;
#5268 = EDGE_CURVE ( 'NONE', #11647, #17860, #729, .T. ) ;
#5269 = CARTESIAN_POINT ( 'NONE',  ( -5.098183173375419486, 20.66060904160994127, -136.0552959529885015 ) ) ;
#5270 = AXIS2_PLACEMENT_3D ( 'NONE', #6511, #15429, #19233 ) ;
#5271 = ORIENTED_EDGE ( 'NONE', *, *, #150, .F. ) ;
#5272 = CARTESIAN_POINT ( 'NONE',  ( -4.683324139160000676, 37.83302525630000446, -140.3020749749999823 ) ) ;
#5273 = DIRECTION ( 'NONE',  ( 2.507771768019999718E-12, 1.592654864069999939E-17, -1.000000000000000000 ) ) ;
#5274 = CIRCLE ( 'NONE', #18944, 6.000000000000001776 ) ;
#5275 = ORIENTED_EDGE ( 'NONE', *, *, #3849, .T. ) ;
#5276 = CARTESIAN_POINT ( 'NONE',  ( -9.157754307290000284, -15.75963164970000108, -147.5552959529999839 ) ) ;
#5277 = VECTOR ( 'NONE', #9617, 1000.000000000000000 ) ;
#5278 = VECTOR ( 'NONE', #16659, 1000.000000000000000 ) ;
#5279 = ADVANCED_FACE ( 'NONE', ( #8157 ), #10055, .T. ) ;
#5280 = CARTESIAN_POINT ( 'NONE',  ( 20.50000000000000000, 25.50000000000000000, -150.0552959529999839 ) ) ;
#5281 = CARTESIAN_POINT ( 'NONE',  ( -13.53810979399600001, -43.39038688405765498, -150.0552959530000123 ) ) ;
#5282 = FACE_OUTER_BOUND ( 'NONE', #2510, .T. ) ;
#5283 = CARTESIAN_POINT ( 'NONE',  ( 19.13369214859999801, -50.50000000000000000, -143.0552959529999839 ) ) ;
#5284 = FACE_OUTER_BOUND ( 'NONE', #4930, .T. ) ;
#5285 = SHAPE_DEFINITION_REPRESENTATION ( #15616, #6919 ) ;
#5286 = CARTESIAN_POINT ( 'NONE',  ( 19.13369214859999801, 51.00000000000000000, -136.0552959530000123 ) ) ;
#5287 = CARTESIAN_POINT ( 'NONE',  ( -6.165211177139999776, -15.11551140080000089, -142.5552959529999839 ) ) ;
#5288 = VECTOR ( 'NONE', #15144, 1000.000000000000000 ) ;
#5289 = ADVANCED_FACE ( 'NONE', ( #19008 ), #22819, .F. ) ;
#5290 = CARTESIAN_POINT ( 'NONE',  ( 8.750000000030000891, -39.98606797749999942, -137.0552959530000123 ) ) ;
#5291 = VECTOR ( 'NONE', #2895, 1000.000000000000000 ) ;
#5292 = VERTEX_POINT ( 'NONE', #12211 ) ;
#5293 = CIRCLE ( 'NONE', #17453, 15.00000000000000000 ) ;
#5294 = ORIENTED_EDGE ( 'NONE', *, *, #9665, .T. ) ;
#5295 = CIRCLE ( 'NONE', #21655, 2.000000000000000000 ) ;
#5296 = CONICAL_SURFACE ( 'NONE', #21657, 1.999999999999992450, 0.7853981633970000820 ) ;
#5297 = ORIENTED_EDGE ( 'NONE', *, *, #9701, .T. ) ;
#5298 = DIRECTION ( 'NONE',  ( -2.257157423930000049E-12, 0.000000000000000000, -1.000000000000000000 ) ) ;
#5299 = CARTESIAN_POINT ( 'NONE',  ( -32.50000000000000000, 28.00000000000000000, -146.5552959529999839 ) ) ;
#5300 = EDGE_CURVE ( 'NONE', #2454, #17032, #4610, .T. ) ;
#5301 = LINE ( 'NONE', #80, #15337 ) ;
#5302 = EDGE_LOOP ( 'NONE', ( #15112, #22922, #17589, #6132 ) ) ;
#5303 = PLANE ( 'NONE',  #11503 ) ;
#5304 = CARTESIAN_POINT ( 'NONE',  ( -19.42944164597027523, 34.87483979447872429, -147.2857474030845424 ) ) ;
#5305 = CARTESIAN_POINT ( 'NONE',  ( -12.41698512492444095, 36.98746477265328991, -147.4237781434714520 ) ) ;
#5306 = LINE ( 'NONE', #14239, #17777 ) ;
#5307 = EDGE_LOOP ( 'NONE', ( #8003, #11184, #15954, #13358 ) ) ;
#5308 = CARTESIAN_POINT ( 'NONE',  ( 7.481747704286809686, 12.99999999999999645, -136.0552959530022008 ) ) ;
#5309 = VECTOR ( 'NONE', #15433, 1000.000000000000000 ) ;
#5310 = ORIENTED_EDGE ( 'NONE', *, *, #19049, .T. ) ;
#5311 = EDGE_CURVE ( 'NONE', #13247, #17813, #19487, .T. ) ;
#5312 = AXIS2_PLACEMENT_3D ( 'NONE', #8547, #7255, #6894 ) ;
#5313 = DIRECTION ( 'NONE',  ( 1.211690350419999855E-27, 2.765629237170000203E-27, -1.000000000000000000 ) ) ;
#5314 = CIRCLE ( 'NONE', #8341, 1.500000000000001332 ) ;
#5315 = EDGE_CURVE ( 'NONE', #23517, #18273, #6623, .T. ) ;
#5316 = VECTOR ( 'NONE', #9696, 1000.000000000000114 ) ;
#5317 = CARTESIAN_POINT ( 'NONE',  ( 13.13369214870000157, 50.50000000000000000, -137.0552959530000123 ) ) ;
#5318 = VECTOR ( 'NONE', #15565, 1000.000000000000000 ) ;
#5319 = AXIS2_PLACEMENT_3D ( 'NONE', #13547, #21299, #23076 ) ;
#5320 = FACE_OUTER_BOUND ( 'NONE', #17317, .T. ) ;
#5321 = ORIENTED_EDGE ( 'NONE', *, *, #19563, .F. ) ;
#5322 = ADVANCED_FACE ( 'NONE', ( #4724 ), #20922, .T. ) ;
#5323 = ADVANCED_FACE ( 'NONE', ( #13884 ), #10416, .T. ) ;
#5324 = CYLINDRICAL_SURFACE ( 'NONE', #20564, 35.00000000000002132 ) ;
#5325 = ORIENTED_EDGE ( 'NONE', *, *, #4922, .T. ) ;
#5326 = CARTESIAN_POINT ( 'NONE',  ( -19.14899212251034299, 37.07484167171372746, -147.8220480109189054 ) ) ;
#5327 = CARTESIAN_POINT ( 'NONE',  ( -32.50000000000000000, -1.000000000000000000, -140.0552959529999839 ) ) ;
#5328 = EDGE_CURVE ( 'NONE', #4355, #3527, #13520, .T. ) ;
#5329 = EDGE_LOOP ( 'NONE', ( #17673, #19947, #5172, #5455, #22802, #18163, #5335, #629, #6248, #5793, #13808, #4278, #4421, #11355, #853, #17481, #20909 ) ) ;
#5330 = CARTESIAN_POINT ( 'NONE',  ( -6.083910486889999802, -15.16899799649999991, -144.5552959529999839 ) ) ;
#5331 = VERTEX_POINT ( 'NONE', #11727 ) ;
#5332 = CARTESIAN_POINT ( 'NONE',  ( -22.00705883600000234, 37.05789963359999462, -148.1619053240000028 ) ) ;
#5333 = EDGE_CURVE ( 'NONE', #16928, #2852, #10767, .T. ) ;
#5334 = DIRECTION ( 'NONE',  ( 0.9989565318111731651, 0.04567108003750790235, -1.889135246290330374E-13 ) ) ;
#5335 = ORIENTED_EDGE ( 'NONE', *, *, #8346, .F. ) ;
#5336 = DIRECTION ( 'NONE',  ( 1.000000000000000000, 0.000000000000000000, 0.000000000000000000 ) ) ;
#5337 = VECTOR ( 'NONE', #2453, 1000.000000000000000 ) ;
#5338 = AXIS2_PLACEMENT_3D ( 'NONE', #901, #2682, #8371 ) ;
#5339 = ORIENTED_EDGE ( 'NONE', *, *, #23349, .T. ) ;
#5340 = AXIS2_PLACEMENT_3D ( 'NONE', #23153, #16134, #3394 ) ;
#5341 = CARTESIAN_POINT ( 'NONE',  ( -25.74743564683659969, 37.94517732363827633, -139.7356315996115939 ) ) ;
#5342 = DIRECTION ( 'NONE',  ( 0.000000000000000000, 1.000000000000000000, 0.000000000000000000 ) ) ;
#5343 = ORIENTED_EDGE ( 'NONE', *, *, #10084, .F. ) ;
#5344 = LINE ( 'NONE', #1670, #17 ) ;
#5345 = CARTESIAN_POINT ( 'NONE',  ( 13.13369214870000157, -2.273736754430000208E-12, -136.0552959530000123 ) ) ;
#5346 = PLANE ( 'NONE',  #723 ) ;
#5347 = ORIENTED_EDGE ( 'NONE', *, *, #6481, .F. ) ;
#5348 = CARTESIAN_POINT ( 'NONE',  ( -15.57039528540000006, 36.22627288620000030, -147.5570433400000070 ) ) ;
#5349 = ORIENTED_EDGE ( 'NONE', *, *, #17458, .T. ) ;
#5350 = VECTOR ( 'NONE', #9725, 1000.000000000000000 ) ;
#5351 = CIRCLE ( 'NONE', #20175, 5.999999999999998224 ) ;
#5352 = CARTESIAN_POINT ( 'NONE',  ( 7.200097415480000151, -13.39991276200000136, -144.5552959529999839 ) ) ;
#5353 = DIRECTION ( 'NONE',  ( -1.211690350419999855E-27, -2.765629237170000203E-27, 1.000000000000000000 ) ) ;
#5354 = EDGE_CURVE ( 'NONE', #22094, #11647, #9055, .T. ) ;
#5355 = FACE_OUTER_BOUND ( 'NONE', #16430, .T. ) ;
#5356 = CARTESIAN_POINT ( 'NONE',  ( -29.04405754857383926, 38.20917013906876036, -139.5702141475971985 ) ) ;
#5357 = ORIENTED_EDGE ( 'NONE', *, *, #13877, .F. ) ;
#5358 = DIRECTION ( 'NONE',  ( 1.000000000000000000, 0.000000000000000000, 0.000000000000000000 ) ) ;
#5359 = DIRECTION ( 'NONE',  ( -1.000000000000000000, 0.000000000000000000, 0.000000000000000000 ) ) ;
#5360 = DIRECTION ( 'NONE',  ( 0.7633862853691523176, -0.6459422414661291079, 0.000000000000000000 ) ) ;
#5361 = DIRECTION ( 'NONE',  ( -0.9980143568310856361, 0.06298685227120542907, 4.509810669690391193E-12 ) ) ;
#5362 = DIRECTION ( 'NONE',  ( -1.456612608300000016E-12, 1.733724275239999964E-12, 1.000000000000000000 ) ) ;
#5363 = LINE ( 'NONE', #14529, #12484 ) ;
#5364 = VERTEX_POINT ( 'NONE', #18048 ) ;
#5365 = CARTESIAN_POINT ( 'NONE',  ( -30.49999999990000177, 47.50000000000000000, -139.8052959529999839 ) ) ;
#5366 = LINE ( 'NONE', #1693, #17487 ) ;
#5367 = CARTESIAN_POINT ( 'NONE',  ( 1.500000000000000000, -3.892699081698731245, -150.0552959530000123 ) ) ;
#5368 = CARTESIAN_POINT ( 'NONE',  ( -5.251527070960000820, 40.93408815870000694, -143.6492421949999994 ) ) ;
#5369 = AXIS2_PLACEMENT_3D ( 'NONE', #6275, #13783, #17460 ) ;
#5370 = CARTESIAN_POINT ( 'NONE',  ( 5.276897646250000129, -21.39828525539999760, -145.5552959529999839 ) ) ;
#5371 = VECTOR ( 'NONE', #12516, 1000.000000000000000 ) ;
#5372 = ORIENTED_EDGE ( 'NONE', *, *, #2567, .F. ) ;
#5373 = FACE_OUTER_BOUND ( 'NONE', #1743, .T. ) ;
#5374 = CARTESIAN_POINT ( 'NONE',  ( -6.083910486889999802, -15.16899799649999991, -145.5552959529999839 ) ) ;
#5375 = ORIENTED_EDGE ( 'NONE', *, *, #13273, .F. ) ;
#5376 = EDGE_CURVE ( 'NONE', #8910, #10616, #22961, .T. ) ;
#5377 = CARTESIAN_POINT ( 'NONE',  ( 4.500000000009999113, -2.000000000000000000, -136.0552959530000123 ) ) ;
#5378 = VERTEX_POINT ( 'NONE', #196 ) ;
#5379 = CARTESIAN_POINT ( 'NONE',  ( -23.90890255102420525, 36.92681688278783270, -147.8857207497513855 ) ) ;
#5380 = EDGE_CURVE ( 'NONE', #15072, #22346, #7439, .T. ) ;
#5381 = DIRECTION ( 'NONE',  ( -8.955190032050000935E-12, 9.104778821549999739E-13, -1.000000000000000000 ) ) ;
#5382 = DIRECTION ( 'NONE',  ( -0.7071067811870332953, 0.000000000000000000, 0.7071067811860618502 ) ) ;
#5383 = CARTESIAN_POINT ( 'NONE',  ( 7.277539027747931932, 37.86935047857989645, -141.7113041814175745 ) ) ;
#5384 = EDGE_LOOP ( 'NONE', ( #17697, #4555, #4258, #11350 ) ) ;
#5385 = DIRECTION ( 'NONE',  ( 1.000000000000000000, 2.602084704489999637E-17, -1.701177084980000217E-20 ) ) ;
#5386 = AXIS2_PLACEMENT_3D ( 'NONE', #740, #20373, #18464 ) ;
#5387 = CARTESIAN_POINT ( 'NONE',  ( -18.82091118372255778, 33.23810407352063834, -144.5979112941300286 ) ) ;
#5388 = VECTOR ( 'NONE', #21145, 1000.000000000000000 ) ;
#5389 = CARTESIAN_POINT ( 'NONE',  ( -9.032885736896121287, 36.94161628545217724, -147.5965110584316164 ) ) ;
#5390 = CARTESIAN_POINT ( 'NONE',  ( -21.35824191589999899, -32.00000000000000000, -144.8157682190000060 ) ) ;
#5391 = VERTEX_POINT ( 'NONE', #9325 ) ;
#5392 = CYLINDRICAL_SURFACE ( 'NONE', #11041, 14.99999999999999645 ) ;
#5393 = B_SPLINE_CURVE_WITH_KNOTS ( 'NONE', 3,
 ( #9054, #8831, #20154, #10965, #16111, #5510, #7056, #14316, #3727, #21588, #16343, #21826, #5269, #1725, #18248, #12522, #8945, #19802 ),
 .UNSPECIFIED., .F., .F.,
 ( 4, 2, 2, 2, 2, 2, 2, 2, 4 ),
 ( 0.000000000000000000, 0.1250000000000000000, 0.2500000000000000000, 0.3750000000000000000, 0.5000000000000000000, 0.6250000000000000000, 0.7500000000000000000, 0.8750000000000000000, 1.000000000000000000 ),
 .UNSPECIFIED. ) ;
#5394 = ORIENTED_EDGE ( 'NONE', *, *, #13587, .T. ) ;
#5395 = CARTESIAN_POINT ( 'NONE',  ( -30.49999999990000177, 27.75000000000000000, -140.5552959529999839 ) ) ;
#5396 = CARTESIAN_POINT ( 'NONE',  ( -6.909346445769999789, 37.92300339060000169, -148.1333867879999957 ) ) ;
#5397 = PLANE ( 'NONE',  #2455 ) ;
#5398 =( BOUNDED_CURVE ( )  B_SPLINE_CURVE ( 5, ( #11521, #606, #13088, #17008, #14995, #20474 ),
 .UNSPECIFIED., .F., .F. ) 
 B_SPLINE_CURVE_WITH_KNOTS ( ( 6, 6 ),
 ( 1.570796326526077813, 3.141592653590000062 ),
 .UNSPECIFIED. ) 
 CURVE ( )  GEOMETRIC_REPRESENTATION_ITEM ( )  RATIONAL_B_SPLINE_CURVE ( ( 0.2500000000000000555, 0.2499999999657597782, 0.2999999999486396840, 0.3999999999315195232, 0.5999999999315195343, 1.000000000000000000 ) ) 
 REPRESENTATION_ITEM ( '' )  );
#5399 = ORIENTED_EDGE ( 'NONE', *, *, #784, .F. ) ;
#5400 = DIRECTION ( 'NONE',  ( -0.09606172499277226828, -0.9953753789357124848, 8.265980492677616040E-13 ) ) ;
#5401 = CARTESIAN_POINT ( 'NONE',  ( -37.89633983739999934, 47.50000000000000000, -139.8120018070000015 ) ) ;
#5402 = MECHANICAL_DESIGN_GEOMETRIC_PRESENTATION_REPRESENTATION (  '', ( #21752 ), #21377 ) ;
#5403 = CIRCLE ( 'NONE', #10311, 0.7500000000000006661 ) ;
#5404 = EDGE_LOOP ( 'NONE', ( #14480, #6053, #2018, #11835 ) ) ;
#5405 = AXIS2_PLACEMENT_3D ( 'NONE', #3368, #5621, #3725 ) ;
#5406 = CARTESIAN_POINT ( 'NONE',  ( -17.89449017629999616, 39.21037955089999372, -147.0820833679999851 ) ) ;
#5407 = LINE ( 'NONE', #12405, #6797 ) ;
#5408 = CARTESIAN_POINT ( 'NONE',  ( 20.50000000000000000, 19.50000000000000000, -136.5552959530000123 ) ) ;
#5409 = B_SPLINE_CURVE_WITH_KNOTS ( 'NONE', 3,
 ( #7100, #8409, #15788, #19367, #17585, #14000, #1297, #21274, #23053, #4968 ),
 .UNSPECIFIED., .F., .F.,
 ( 4, 2, 2, 2, 4 ),
 ( 0.000000000000000000, 0.2500000000000000000, 0.5000000000000000000, 0.7500000000000000000, 1.000000000000000000 ),
 .UNSPECIFIED. ) ;
#5410 = LINE ( 'NONE', #18136, #8363 ) ;
#5411 = ADVANCED_FACE ( 'NONE', ( #16599 ), #15397, .F. ) ;
#5412 = CYLINDRICAL_SURFACE ( 'NONE', #8201, 1.500000000000001998 ) ;
#5413 = CARTESIAN_POINT ( 'NONE',  ( -17.18002735256250446, 36.98113687425440332, -140.6755148967336595 ) ) ;
#5414 = PLANE ( 'NONE',  #14313 ) ;
#5415 = EDGE_CURVE ( 'NONE', #5167, #21713, #1495, .T. ) ;
#5416 = FACE_OUTER_BOUND ( 'NONE', #21070, .T. ) ;
#5417 = DIRECTION ( 'NONE',  ( 2.257157423930000049E-12, 0.000000000000000000, 1.000000000000000000 ) ) ;
#5418 = ORIENTED_EDGE ( 'NONE', *, *, #6634, .F. ) ;
#5419 = STYLED_ITEM ( 'NONE', ( #7198 ), #18583 ) ;
#5420 = PRODUCT_DEFINITION_CONTEXT ( 'detailed design', #14356, 'design' ) ;
#5421 = VECTOR ( 'NONE', #14615, 1000.000000000000000 ) ;
#5422 = ORIENTED_EDGE ( 'NONE', *, *, #10406, .F. ) ;
#5423 = EDGE_LOOP ( 'NONE', ( #22931, #14893, #717, #3015 ) ) ;
#5424 = FACE_OUTER_BOUND ( 'NONE', #12549, .T. ) ;
#5425 = CARTESIAN_POINT ( 'NONE',  ( -12.56920363940049512, 37.00563451942266369, -148.6543378380284821 ) ) ;
#5426 = ORIENTED_EDGE ( 'NONE', *, *, #7638, .F. ) ;
#5427 = CARTESIAN_POINT ( 'NONE',  ( 14.00000000000001421, 20.99298601554737331, -136.0552959530316173 ) ) ;
#5428 = ORIENTED_EDGE ( 'NONE', *, *, #16317, .T. ) ;
#5429 = LINE ( 'NONE', #8741, #6821 ) ;
#5430 = CARTESIAN_POINT ( 'NONE',  ( -15.50000000000000000, 47.50000000000000000, -150.5552959529999839 ) ) ;
#5431 = CARTESIAN_POINT ( 'NONE',  ( -12.04808041671338081, 40.71874701608464164, -143.7411651109900106 ) ) ;
#5432 = DIRECTION ( 'NONE',  ( 0.6459422414661299960, 0.7633862853691516515, 0.000000000000000000 ) ) ;
#5433 = EDGE_LOOP ( 'NONE', ( #14124, #12310 ) ) ;
#5434 = CARTESIAN_POINT ( 'NONE',  ( -7.047250123649999587, -34.50000000000000000, -150.0552959529999839 ) ) ;
#5435 = ADVANCED_FACE ( 'NONE', ( #6949 ), #1846, .F. ) ;
#5436 = ORIENTED_EDGE ( 'NONE', *, *, #17963, .F. ) ;
#5437 = CARTESIAN_POINT ( 'NONE',  ( 9.280367625918376717, 35.71890903872555612, -141.9084521930435017 ) ) ;
#5438 = VECTOR ( 'NONE', #13829, 1000.000000000000114 ) ;
#5439 = DIRECTION ( 'NONE',  ( -2.257252162960000001E-12, 0.000000000000000000, -1.000000000000000000 ) ) ;
#5440 = CARTESIAN_POINT ( 'NONE',  ( -7.041959465309999722, -26.08051538799999847, -143.0552959529999839 ) ) ;
#5441 = ADVANCED_FACE ( 'NONE', ( #21476, #8717, #10618, #8954, #9066, #19572 ), #5159, .T. ) ;
#5442 = ORIENTED_EDGE ( 'NONE', *, *, #15525, .F. ) ;
#5443 = CARTESIAN_POINT ( 'NONE',  ( -6.033650297970000409, 36.94170754819999303, -147.9652040070000112 ) ) ;
#5444 = ORIENTED_EDGE ( 'NONE', *, *, #1278, .T. ) ;
#5445 = LINE ( 'NONE', #21516, #17024 ) ;
#5446 = FACE_OUTER_BOUND ( 'NONE', #8558, .T. ) ;
#5447 = ORIENTED_EDGE ( 'NONE', *, *, #2305, .F. ) ;
#5448 = CARTESIAN_POINT ( 'NONE',  ( -25.74974290510757413, 39.24565833955466587, -141.0594917313689791 ) ) ;
#5449 = ORIENTED_EDGE ( 'NONE', *, *, #16484, .F. ) ;
#5450 = CARTESIAN_POINT ( 'NONE',  ( -15.27002291891846042, 38.46844526377296347, -147.3668459616297923 ) ) ;
#5451 = EDGE_CURVE ( 'NONE', #14557, #9232, #18134, .T. ) ;
#5452 = CARTESIAN_POINT ( 'NONE',  ( -32.50000000000000000, 26.00000000000000000, -141.5552959529999839 ) ) ;
#5453 = ORIENTED_EDGE ( 'NONE', *, *, #2409, .F. ) ;
#5454 = DIRECTION ( 'NONE',  ( 0.000000000000000000, 0.000000000000000000, 1.000000000000000000 ) ) ;
#5455 = ORIENTED_EDGE ( 'NONE', *, *, #19894, .F. ) ;
#5456 = CARTESIAN_POINT ( 'NONE',  ( -27.10435930909369517, 40.49789879880128041, -141.9338419167955010 ) ) ;
#5457 = PLANE ( 'NONE',  #20241 ) ;
#5458 = ORIENTED_EDGE ( 'NONE', *, *, #22202, .F. ) ;
#5459 = CYLINDRICAL_SURFACE ( 'NONE', #1157, 4.999999999999999112 ) ;
#5460 = CARTESIAN_POINT ( 'NONE',  ( -10.22994911489607262, 35.59422248375447140, -140.5010413741651689 ) ) ;
#5461 = EDGE_CURVE ( 'NONE', #8637, #12948, #5407, .T. ) ;
#5462 = DIRECTION ( 'NONE',  ( -1.000000000000000000, -2.808280234649999694E-18, -2.507771768019999718E-12 ) ) ;
#5463 = ORIENTED_EDGE ( 'NONE', *, *, #3986, .F. ) ;
#5464 = ADVANCED_FACE ( 'NONE', ( #19808 ), #15994, .T. ) ;
#5465 = CARTESIAN_POINT ( 'NONE',  ( -13.91784526140000011, 35.46792342009999288, -140.7554205120000006 ) ) ;
#5466 = EDGE_CURVE ( 'NONE', #14773, #2149, #17560, .T. ) ;
#5467 = DIRECTION ( 'NONE',  ( 0.000000000000000000, -1.000000000000000000, 8.159623473500000156E-13 ) ) ;
#5468 = ADVANCED_FACE ( 'NONE', ( #16234 ), #10389, .F. ) ;
#5469 = ORIENTED_EDGE ( 'NONE', *, *, #8630, .F. ) ;
#5470 = CARTESIAN_POINT ( 'NONE',  ( -9.934356875269999776, -23.16624500709999879, -145.5552959529999839 ) ) ;
#5471 = FACE_OUTER_BOUND ( 'NONE', #13086, .T. ) ;
#5472 = CARTESIAN_POINT ( 'NONE',  ( -17.75130813170000366, 41.00325609940000504, -141.6328284839999867 ) ) ;
#5473 = CARTESIAN_POINT ( 'NONE',  ( -22.21135766849999982, 35.30661492690000358, -147.9492090369999744 ) ) ;
#5474 = EDGE_LOOP ( 'NONE', ( #21908, #2254, #20686, #10327, #9134 ) ) ;
#5475 = DIRECTION ( 'NONE',  ( 0.000000000000000000, -1.000000000000000000, 0.000000000000000000 ) ) ;
#5476 = CARTESIAN_POINT ( 'NONE',  ( -6.603585321229999749, -20.59801339440000234, -143.5552959529999839 ) ) ;
#5477 = DIRECTION ( 'NONE',  ( 0.000000000000000000, -1.000000000000000000, 0.000000000000000000 ) ) ;
#5478 = LINE ( 'NONE', #11274, #19388 ) ;
#5479 = DIRECTION ( 'NONE',  ( 1.000000000000000000, 2.602084704489999637E-17, -2.257171095940000041E-12 ) ) ;
#5480 = DIRECTION ( 'NONE',  ( 1.000000000000000000, 2.602084704489999637E-17, -1.701177084980000217E-20 ) ) ;
#5481 = ORIENTED_EDGE ( 'NONE', *, *, #8283, .F. ) ;
#5482 = CARTESIAN_POINT ( 'NONE',  ( 2.139623390130000136, -12.81320239329999922, -143.5552959529999839 ) ) ;
#5483 = LINE ( 'NONE', #1578, #20173 ) ;
#5484 = CARTESIAN_POINT ( 'NONE',  ( 1.500000000000000000, -3.500000000000000000, -150.0552959529999839 ) ) ;
#5485 = CARTESIAN_POINT ( 'NONE',  ( -6.622935940118527931, 39.79829474619231888, -147.7685723067526737 ) ) ;
#5486 = CARTESIAN_POINT ( 'NONE',  ( -14.07817992003762697, -44.19950026359727957, -136.0552959530021155 ) ) ;
#5487 = ORIENTED_EDGE ( 'NONE', *, *, #17383, .F. ) ;
#5488 = EDGE_CURVE ( 'NONE', #3279, #17827, #23139, .T. ) ;
#5489 = AXIS2_PLACEMENT_3D ( 'NONE', #2680, #9906, #13604 ) ;
#5490 = CARTESIAN_POINT ( 'NONE',  ( -27.77832206610000298, 37.03059619289999915, -147.6270870419999710 ) ) ;
#5491 = EDGE_CURVE ( 'NONE', #22206, #11516, #21646, .T. ) ;
#5492 = CARTESIAN_POINT ( 'NONE',  ( -21.03694116389999635, 36.94210036639999828, -147.9486865819999935 ) ) ;
#5493 = ORIENTED_EDGE ( 'NONE', *, *, #23043, .T. ) ;
#5494 = CARTESIAN_POINT ( 'NONE',  ( -26.33255611194163137, 36.96293009473755831, -139.4434112040621585 ) ) ;
#5495 = VERTEX_POINT ( 'NONE', #14569 ) ;
#5496 = CARTESIAN_POINT ( 'NONE',  ( 6.500000000149999124, 20.50000000000000000, -143.5552959529999839 ) ) ;
#5497 = CARTESIAN_POINT ( 'NONE',  ( -29.57813679455983902, 37.90625934871609815, -140.4594347136643080 ) ) ;
#5498 = CARTESIAN_POINT ( 'NONE',  ( -21.13851658209999940, 36.11334442980000148, -147.9366295160000107 ) ) ;
#5499 = CARTESIAN_POINT ( 'NONE',  ( 7.653144819507610386, 38.23813455914281434, -141.8834125977530221 ) ) ;
#5500 = ORIENTED_EDGE ( 'NONE', *, *, #6889, .F. ) ;
#5501 = CARTESIAN_POINT ( 'NONE',  ( -11.65594158663979485, 36.92432879709620863, -140.1042033537094085 ) ) ;
#5502 = CARTESIAN_POINT ( 'NONE',  ( -20.45144833149999997, 36.94873838139999833, -139.8044047869999815 ) ) ;
#5503 = LINE ( 'NONE', #16335, #6761 ) ;
#5504 = LINE ( 'NONE', #12751, #11442 ) ;
#5505 = VERTEX_POINT ( 'NONE', #16573 ) ;
#5506 = LINE ( 'NONE', #12754, #4616 ) ;
#5507 = ORIENTED_EDGE ( 'NONE', *, *, #17299, .T. ) ;
#5508 = CARTESIAN_POINT ( 'NONE',  ( 6.750000000030000002, -33.75000000000000000, -136.0552959530000123 ) ) ;
#5509 = DIRECTION ( 'NONE',  ( 4.510774274160000731E-12, -1.321907670990000086E-13, 1.000000000000000000 ) ) ;
#5510 = CARTESIAN_POINT ( 'NONE',  ( -5.098088255135088787, 24.33948587670753128, -136.0552959529885015 ) ) ;
#5511 = ORIENTED_EDGE ( 'NONE', *, *, #22750, .F. ) ;
#5512 = ADVANCED_FACE ( 'NONE', ( #9297 ), #20163, .F. ) ;
#5513 = CARTESIAN_POINT ( 'NONE',  ( -6.599926022991117414, 40.46602300537465879, -145.9459310978139968 ) ) ;
#5514 = CARTESIAN_POINT ( 'NONE',  ( 4.352290413739999586, -26.01556969399999986, -146.5552959529999839 ) ) ;
#5515 = ORIENTED_EDGE ( 'NONE', *, *, #9632, .F. ) ;
#5516 = FACE_OUTER_BOUND ( 'NONE', #12806, .T. ) ;
#5517 = DIRECTION ( 'NONE',  ( -2.602084747549999882E-17, 1.000000000000000000, 5.873289694040000105E-29 ) ) ;
#5519 = VECTOR ( 'NONE', #20102, 1000.000000000000000 ) ;
#5518 = CARTESIAN_POINT ( 'NONE',  ( -12.50000000000000000, 25.50000000000000000, -136.0552959530000123 ) ) ;
#5520 = CARTESIAN_POINT ( 'NONE',  ( -25.20835066603357433, 36.21492759592103283, -148.1779083850792915 ) ) ;
#5521 = CARTESIAN_POINT ( 'NONE',  ( -6.477935707790000386, -19.20465386649999928, -146.5552959529999839 ) ) ;
#5522 = FACE_OUTER_BOUND ( 'NONE', #11754, .T. ) ;
#5523 = ITEM_DEFINED_TRANSFORMATION ( 'NONE', 'NONE', #23314,  #5025 ) ;
#5524 = LINE ( 'NONE', #5164, #10885 ) ;
#5525 = CARTESIAN_POINT ( 'NONE',  ( 1.000000000140000012, 36.50000000000000000, -147.5552959529999839 ) ) ;
#5526 = DIRECTION ( 'NONE',  ( -0.7633862853691524286, -0.6459422414661293299, 0.000000000000000000 ) ) ;
#5527 = EDGE_LOOP ( 'NONE', ( #10291, #1279, #20177, #9571 ) ) ;
#5528 =( BOUNDED_CURVE ( )  B_SPLINE_CURVE ( 5, ( #1361, #20032, #7297, #19561, #19672, #21356, #10729, #19914, #6819, #5046, #5396, #3254 ),
 .UNSPECIFIED., .F., .F. ) 
 B_SPLINE_CURVE_WITH_KNOTS ( ( 6, 3, 3, 6 ),
 ( 0.000000000000000000, 4.445608688430000122, 8.917804078430000558, 13.41780914199999941 ),
 .UNSPECIFIED. ) 
 CURVE ( )  GEOMETRIC_REPRESENTATION_ITEM ( )  RATIONAL_B_SPLINE_CURVE ( ( 0.2500000000000000000, 0.2500000000000000000, 0.2500000000000000000, 0.2500000000000000000, 0.2500000000000000000, 0.2500000000000000000, 0.2500000000000000000, 0.2500000000000000000, 0.2500000000000000000, 0.2500000000000000000, 0.2500000000000000000, 0.2500000000000000000 ) ) 
 REPRESENTATION_ITEM ( '' )  );
#5529 = EDGE_LOOP ( 'NONE', ( #8370, #9237, #14934, #2807 ) ) ;
#5530 = SURFACE_STYLE_FILL_AREA ( #19933 ) ;
#5531 = ORIENTED_EDGE ( 'NONE', *, *, #9466, .T. ) ;
#5532 = VECTOR ( 'NONE', #8091, 1000.000000000000000 ) ;
#5533 = CARTESIAN_POINT ( 'NONE',  ( -17.02323386554646589, 33.09469489192927938, -141.6593809025141013 ) ) ;
#5534 = CARTESIAN_POINT ( 'NONE',  ( 32.50000000000000000, -39.80430157320000006, -149.5552959529999839 ) ) ;
#5535 = ORIENTED_EDGE ( 'NONE', *, *, #6029, .T. ) ;
#5536 = VECTOR ( 'NONE', #17425, 1000.000000000000000 ) ;
#5537 = CARTESIAN_POINT ( 'NONE',  ( 6.500000000040000003, 28.00000000000000000, -136.0552959530000123 ) ) ;
#5538 = ORIENTED_EDGE ( 'NONE', *, *, #17213, .T. ) ;
#5539 = ADVANCED_FACE ( 'NONE', ( #7413 ), #3734, .T. ) ;
#5540 = DIRECTION ( 'NONE',  ( 1.000000000000000000, -5.094701932209999624E-24, -2.257144641399999941E-12 ) ) ;
#5541 = CARTESIAN_POINT ( 'NONE',  ( -20.13043194029999938, 34.25277599949999541, -140.5881547479999938 ) ) ;
#5542 = ADVANCED_FACE ( 'NONE', ( #12883 ), #20039, .F. ) ;
#5543 = DIRECTION ( 'NONE',  ( -5.094701932209999624E-24, -1.000000000000000000, 1.149947916579999802E-35 ) ) ;
#5544 = ORIENTED_EDGE ( 'NONE', *, *, #1110, .T. ) ;
#5545 = CARTESIAN_POINT ( 'NONE',  ( 32.00000000000000000, -21.03620104879999886, -136.0552959530000123 ) ) ;
#5546 = ORIENTED_EDGE ( 'NONE', *, *, #9010, .T. ) ;
#5547 = CARTESIAN_POINT ( 'NONE',  ( 8.962004831856564380, 35.57270853839675340, -142.0027968019423383 ) ) ;
#5548 = CYLINDRICAL_SURFACE ( 'NONE', #2874, 7.000000000000000888 ) ;
#5549 = AXIS2_PLACEMENT_3D ( 'NONE', #6051, #15332, #18783 ) ;
#5550 = LINE ( 'NONE', #12797, #8991 ) ;
#5551 = VECTOR ( 'NONE', #9515, 1000.000000000000000 ) ;
#5552 = ORIENTED_EDGE ( 'NONE', *, *, #3201, .T. ) ;
#5553 = DIRECTION ( 'NONE',  ( 0.000000000000000000, -1.000000000000000000, 0.000000000000000000 ) ) ;
#5554 = ORIENTED_EDGE ( 'NONE', *, *, #12858, .T. ) ;
#5555 = CARTESIAN_POINT ( 'NONE',  ( 7.270619713743966983, -48.94911951120975857, -150.0552959529999839 ) ) ;
#5556 = CARTESIAN_POINT ( 'NONE',  ( 24.36715301250000110, -30.57462384669999977, -147.0552959529999839 ) ) ;
#5557 = EDGE_LOOP ( 'NONE', ( #18380, #23419, #10749, #10381 ) ) ;
#5558 = CARTESIAN_POINT ( 'NONE',  ( -25.99376360891585236, 38.42570013690371411, -140.8815290731379832 ) ) ;
#5559 = VERTEX_POINT ( 'NONE', #3855 ) ;
#5560 = CARTESIAN_POINT ( 'NONE',  ( -23.22979221369066849, 36.01619379403584276, -139.4644529137362952 ) ) ;
#5561 = CARTESIAN_POINT ( 'NONE',  ( 8.500000000060001781, 35.50000000000000000, -142.0552959529999839 ) ) ;
#5562 = EDGE_LOOP ( 'NONE', ( #12905, #7273, #4745, #14833 ) ) ;
#5563 = APPLICATION_PROTOCOL_DEFINITION ( 'draft international standard', 'automotive_design', 1998, #9918 ) ;
#5564 = ORIENTED_EDGE ( 'NONE', *, *, #4657, .T. ) ;
#5565 = DIRECTION ( 'NONE',  ( 1.000000000000000000, 0.000000000000000000, -2.257120985840000117E-12 ) ) ;
#5566 = VECTOR ( 'NONE', #2918, 1000.000000000000000 ) ;
#5567 = PLANE ( 'NONE',  #8446 ) ;
#5568 = EDGE_CURVE ( 'NONE', #6870, #2237, #11092, .T. ) ;
#5569 = LINE ( 'NONE', #3439, #6840 ) ;
#5570 = CARTESIAN_POINT ( 'NONE',  ( -10.14672265977482191, 34.69385710102684328, -140.5370343418454979 ) ) ;
#5571 = LINE ( 'NONE', #12345, #16296 ) ;
#5572 = EDGE_LOOP ( 'NONE', ( #1665, #1510, #19486, #7506 ) ) ;
#5573 = CARTESIAN_POINT ( 'NONE',  ( 25.50000000000000000, 25.50000000000000000, -150.0552959529999839 ) ) ;
#5574 = CARTESIAN_POINT ( 'NONE',  ( 8.500000000060001781, 35.50000000000000000, -146.0552959529999839 ) ) ;
#5575 = EDGE_CURVE ( 'NONE', #13874, #990, #4920, .T. ) ;
#5576 = ORIENTED_EDGE ( 'NONE', *, *, #19428, .T. ) ;
#5577 = PLANE ( 'NONE',  #8982 ) ;
#5578 = LINE ( 'NONE', #18321, #22999 ) ;
#5579 = FACE_BOUND ( 'NONE', #14822, .T. ) ;
#5580 = CARTESIAN_POINT ( 'NONE',  ( -29.36003260549882654, 40.56893091388222672, -146.2070596150487916 ) ) ;
#5581 = VECTOR ( 'NONE', #17669, 1000.000000000000000 ) ;
#5582 = ORIENTED_EDGE ( 'NONE', *, *, #23057, .T. ) ;
#5583 = CARTESIAN_POINT ( 'NONE',  ( -13.86630785140000022, 50.50000000000000000, -137.0552959530000123 ) ) ;
#5584 = CARTESIAN_POINT ( 'NONE',  ( 6.000000000140000012, 29.48610037779999971, -147.5552959529999839 ) ) ;
#5585 = EDGE_CURVE ( 'NONE', #9664, #9123, #9191, .T. ) ;
#5586 = CARTESIAN_POINT ( 'NONE',  ( 25.96278831669999931, 46.03148680889999866, -136.0552959530000123 ) ) ;
#5587 = LINE ( 'NONE', #12835, #12134 ) ;
#5588 = CARTESIAN_POINT ( 'NONE',  ( -17.53224077489999999, 39.64394931100000008, -140.2973660050000149 ) ) ;
#5589 = DIRECTION ( 'NONE',  ( 0.000000000000000000, 1.000000000000000000, 0.000000000000000000 ) ) ;
#5590 = EDGE_LOOP ( 'NONE', ( #9051, #8216 ) ) ;
#5591 = CARTESIAN_POINT ( 'NONE',  ( -27.58442046400475789, 33.75941976971765968, -145.8216020747523487 ) ) ;
#5592 = EDGE_CURVE ( 'NONE', #4919, #20880, #5976, .T. ) ;
#5593 = DIRECTION ( 'NONE',  ( 1.000000000000000000, 0.000000000000000000, 0.000000000000000000 ) ) ;
#5594 = CARTESIAN_POINT ( 'NONE',  ( 2.100999472805463064, -5.343640159924751387, -150.0552959529999839 ) ) ;
#5595 = CARTESIAN_POINT ( 'NONE',  ( -5.038554799627442904, 41.08894039876798843, -141.7131813093625681 ) ) ;
#5596 = LINE ( 'NONE', #5125, #16139 ) ;
#5597 = VECTOR ( 'NONE', #20282, 1000.000000000000000 ) ;
#5598 = ORIENTED_EDGE ( 'NONE', *, *, #21643, .F. ) ;
#5599 = DIRECTION ( 'NONE',  ( 1.000000000000000000, 0.000000000000000000, 0.000000000000000000 ) ) ;
#5600 = FACE_OUTER_BOUND ( 'NONE', #11412, .T. ) ;
#5601 = VERTEX_POINT ( 'NONE', #16927 ) ;
#5602 = EDGE_CURVE ( 'NONE', #21645, #9539, #17282, .T. ) ;
#5603 = ORIENTED_EDGE ( 'NONE', *, *, #20750, .T. ) ;
#5604 = ADVANCED_FACE ( 'NONE', ( #636 ), #4323, .T. ) ;
#5605 = CARTESIAN_POINT ( 'NONE',  ( -23.20965953747223764, 36.97759979273075714, -140.7013664825230705 ) ) ;
#5606 = CARTESIAN_POINT ( 'NONE',  ( -21.71608528380000180, -34.50000000000000000, -144.8157682190000060 ) ) ;
#5607 = CARTESIAN_POINT ( 'NONE',  ( 29.68320006080000084, -16.50000000000000000, -148.5552959529999839 ) ) ;
#5608 = CARTESIAN_POINT ( 'NONE',  ( 22.40528270640000130, -21.39206583629999869, -146.0552959529999839 ) ) ;
#5609 = EDGE_LOOP ( 'NONE', ( #10898, #7639, #10998, #20544, #12176, #3238, #9616 ) ) ;
#5610 = CARTESIAN_POINT ( 'NONE',  ( -11.19828263913021971, 35.50589712243412066, -140.5907466445859768 ) ) ;
#5611 = CARTESIAN_POINT ( 'NONE',  ( -19.38605492674887998, 35.40602226203012037, -140.5130341975410317 ) ) ;
#5612 = AXIS2_PLACEMENT_3D ( 'NONE', #19432, #14073, #17880 ) ;
#5613 = EDGE_CURVE ( 'NONE', #919, #15451, #2661, .T. ) ;
#5614 = LINE ( 'NONE', #12866, #14362 ) ;
#5615 = DIRECTION ( 'NONE',  ( -0.9847555042252370550, 0.1739442350240419932, 0.000000000000000000 ) ) ;
#5616 = DIRECTION ( 'NONE',  ( 2.257157423930000049E-12, 0.000000000000000000, 1.000000000000000000 ) ) ;
#5617 = EDGE_CURVE ( 'NONE', #8763, #70, #18946, .T. ) ;
#5618 = VECTOR ( 'NONE', #9868, 1000.000000000000000 ) ;
#5619 = CARTESIAN_POINT ( 'NONE',  ( -9.282104535860000283, -16.71402168319999859, -145.5552959529999839 ) ) ;
#5620 = EDGE_CURVE ( 'NONE', #23525, #9016, #18831, .T. ) ;
#5621 = DIRECTION ( 'NONE',  ( 1.526468026909999897E-13, 8.159623473500000156E-13, 1.000000000000000000 ) ) ;
#5622 = CARTESIAN_POINT ( 'NONE',  ( 25.31684607429999900, 45.26810052439999765, -150.0552959529999839 ) ) ;
#5623 = DIRECTION ( 'NONE',  ( 1.000000000000000000, 0.000000000000000000, 0.000000000000000000 ) ) ;
#5624 = EDGE_LOOP ( 'NONE', ( #22105, #2816, #2837, #17127, #19060, #2996 ) ) ;
#5625 = CARTESIAN_POINT ( 'NONE',  ( -6.703522560530410068, 37.74709865770818595, -147.4226397534824287 ) ) ;
#5626 = ORIENTED_EDGE ( 'NONE', *, *, #10962, .T. ) ;
#5627 = SURFACE_STYLE_USAGE ( .BOTH. , #22402 ) ;
#5628 = VECTOR ( 'NONE', #2176, 1000.000000000000000 ) ;
#5629 = DIRECTION ( 'NONE',  ( 0.000000000000000000, 0.000000000000000000, -1.000000000000000000 ) ) ;
#5630 = VECTOR ( 'NONE', #7562, 1000.000000000000227 ) ;
#5631 = DIRECTION ( 'NONE',  ( -1.000000000000000000, 0.000000000000000000, 2.257076750570000197E-12 ) ) ;
#5632 = CARTESIAN_POINT ( 'NONE',  ( -25.07725372939999886, 36.26300138690000097, -147.8685835880000070 ) ) ;
#5633 = CARTESIAN_POINT ( 'NONE',  ( 8.995627988029999855, -17.23072307649999857, -146.5552959529999839 ) ) ;
#5634 = CARTESIAN_POINT ( 'NONE',  ( 13.98537695654772328, 33.88080765319283927, -150.0552959530000123 ) ) ;
#5635 = DIRECTION ( 'NONE',  ( 9.092994329339670690E-12, 0.000000000000000000, 1.000000000000000000 ) ) ;
#5636 = DIRECTION ( 'NONE',  ( 8.740345284041279692E-14, 0.000000000000000000, 1.000000000000000000 ) ) ;
#5637 = DIRECTION ( 'NONE',  ( -2.257144641399999941E-12, 0.000000000000000000, -1.000000000000000000 ) ) ;
#5638 = ORIENTED_EDGE ( 'NONE', *, *, #15794, .T. ) ;
#5639 = EDGE_CURVE ( 'NONE', #18084, #13274, #15547, .T. ) ;
#5640 = UNCERTAINTY_MEASURE_WITH_UNIT (LENGTH_MEASURE( 1.000000000000000082E-05 ), #7720, 'distance_accuracy_value', 'NONE');
#5642 = ORIENTED_EDGE ( 'NONE', *, *, #20887, .F. ) ;
#5641 = AXIS2_PLACEMENT_3D ( 'NONE', #11664, #8104, #9438 ) ;
#5643 = CIRCLE ( 'NONE', #21997, 1.499999999999999556 ) ;
#5644 = VERTEX_POINT ( 'NONE', #8224 ) ;
#5645 = DIRECTION ( 'NONE',  ( 1.000000000000000000, 0.000000000000000000, -2.253752739989067373E-12 ) ) ;
#5646 = LINE ( 'NONE', #16834, #16014 ) ;
#5647 = LINE ( 'NONE', #13025, #9999 ) ;
#5648 = ORIENTED_EDGE ( 'NONE', *, *, #22317, .F. ) ;
#5649 = VECTOR ( 'NONE', #2162, 1000.000000000000000 ) ;
#5650 = DIRECTION ( 'NONE',  ( 0.000000000000000000, 0.000000000000000000, 1.000000000000000000 ) ) ;
#5651 = CARTESIAN_POINT ( 'NONE',  ( -18.91006587252563875, 33.19603641697479190, -143.7906546518351831 ) ) ;
#5652 = DIRECTION ( 'NONE',  ( -1.000000000000000000, -7.105427357600000794E-15, 2.273736754430000208E-12 ) ) ;
#5653 = ORIENTED_EDGE ( 'NONE', *, *, #21592, .T. ) ;
#5654 = FACE_BOUND ( 'NONE', #15792, .T. ) ;
#5655 = CARTESIAN_POINT ( 'NONE',  ( 9.576259528318086467, 38.04486978495457095, -141.7841118833629821 ) ) ;
#5656 = CIRCLE ( 'NONE', #14396, 25.00000000000000000 ) ;
#5657 = CARTESIAN_POINT ( 'NONE',  ( 6.500000000030000002, 13.00000000000000000, -136.5552959530000123 ) ) ;
#5658 = AXIS2_PLACEMENT_3D ( 'NONE', #2268, #9494, #11984 ) ;
#5659 = ORIENTED_EDGE ( 'NONE', *, *, #10981, .T. ) ;
#5660 =( BOUNDED_CURVE ( )  B_SPLINE_CURVE ( 5, ( #8667, #12360, #23442, #1220, #23092, #23327 ),
 .UNSPECIFIED., .F., .F. ) 
 B_SPLINE_CURVE_WITH_KNOTS ( ( 6, 6 ),
 ( 1.570796326712887714, 3.141592653590000062 ),
 .UNSPECIFIED. ) 
 CURVE ( )  GEOMETRIC_REPRESENTATION_ITEM ( )  RATIONAL_B_SPLINE_CURVE ( ( 0.2499999999999999445, 0.2499999999895451408, 0.2999999999843177001, 0.3999999999790902483, 0.5999999999790902594, 1.000000000000000000 ) ) 
 REPRESENTATION_ITEM ( '' )  );
#5661 = AXIS2_PLACEMENT_3D ( 'NONE', #2646, #9876, #8560 ) ;
#5662 = ADVANCED_FACE ( 'NONE', ( #8107 ), #17040, .T. ) ;
#5663 = AXIS2_PLACEMENT_3D ( 'NONE', #17454, #6270, #20677 ) ;
#5664 = CARTESIAN_POINT ( 'NONE',  ( 23.50000000000000000, -20.50000000000000000, -143.5552959529999839 ) ) ;
#5665 = ORIENTED_EDGE ( 'NONE', *, *, #1742, .T. ) ;
#5666 = CARTESIAN_POINT ( 'NONE',  ( 8.496192186297829352, -48.00965300675227354, -150.0552959530000123 ) ) ;
#5667 = ADVANCED_FACE ( 'NONE', ( #22753 ), #10123, .F. ) ;
#5668 = VERTEX_POINT ( 'NONE', #13711 ) ;
#5669 = CARTESIAN_POINT ( 'NONE',  ( -25.56118619078102583, 37.81731597404795764, -140.4616157252740720 ) ) ;
#5670 = EDGE_LOOP ( 'NONE', ( #21435, #2534, #10146, #11717 ) ) ;
#5671 = LINE ( 'NONE', #13157, #4903 ) ;
#5672 = ORIENTED_EDGE ( 'NONE', *, *, #5488, .F. ) ;
#5673 = DIRECTION ( 'NONE',  ( 1.000000000000000000, 0.000000000000000000, 0.000000000000000000 ) ) ;
#5674 = ORIENTED_EDGE ( 'NONE', *, *, #7232, .T. ) ;
#5675 = PRODUCT_CONTEXT ( 'NONE', #7803, 'mechanical' ) ;
#5676 = AXIS2_PLACEMENT_3D ( 'NONE', #10975, #14798, #21834 ) ;
#5677 = EDGE_LOOP ( 'NONE', ( #13252, #18868, #4237 ) ) ;
#5678 = CARTESIAN_POINT ( 'NONE',  ( -27.46357115055653253, 41.16992305278137820, -146.3751964293791730 ) ) ;
#5679 = AXIS2_PLACEMENT_3D ( 'NONE', #20484, #4186, #7396 ) ;
#5680 = CARTESIAN_POINT ( 'NONE',  ( -24.87949572109999963, 37.83967983510000010, -147.8465544160000036 ) ) ;
#5681 = CARTESIAN_POINT ( 'NONE',  ( 10.25767361203778805, 27.00937110137719444, -150.0552959529999839 ) ) ;
#5682 = DIRECTION ( 'NONE',  ( -3.994014902950000436E-29, 1.000000000000000000, -4.148443855749999753E-27 ) ) ;
#5683 = AXIS2_PLACEMENT_3D ( 'NONE', #4959, #12205, #19481 ) ;
#5684 = CARTESIAN_POINT ( 'NONE',  ( -10.32240832042323220, 36.33503176822112124, -140.3275047487922791 ) ) ;
#5685 = AXIS2_PLACEMENT_3D ( 'NONE', #6054, #22591, #4623 ) ;
#5686 = CARTESIAN_POINT ( 'NONE',  ( -8.641895390041296920, 41.79448446390107108, -143.5108926868431638 ) ) ;
#5687 = VERTEX_POINT ( 'NONE', #22527 ) ;
#5688 = DIRECTION ( 'NONE',  ( 0.000000000000000000, 1.000000000000000000, 0.000000000000000000 ) ) ;
#5689 = CARTESIAN_POINT ( 'NONE',  ( 9.169979960837745026, 35.65450163122486771, -146.1628100147027567 ) ) ;
#5690 = ORIENTED_EDGE ( 'NONE', *, *, #21880, .T. ) ;
#5691 = CARTESIAN_POINT ( 'NONE',  ( -15.50000000000000000, 21.50000000000000000, -150.0552959529999839 ) ) ;
#5692 = CARTESIAN_POINT ( 'NONE',  ( -11.21018092005731326, 39.88389201235554538, -140.2749471409629507 ) ) ;
#5693 = EDGE_CURVE ( 'NONE', #2155, #12574, #19182, .T. ) ;
#5694 = FACE_OUTER_BOUND ( 'NONE', #5474, .T. ) ;
#5695 = DIRECTION ( 'NONE',  ( 0.000000000000000000, 0.000000000000000000, 1.000000000000000000 ) ) ;
#5696 = ORIENTED_EDGE ( 'NONE', *, *, #17515, .T. ) ;
#5697 = CARTESIAN_POINT ( 'NONE',  ( -6.713398844220000328, 32.91877557720000169, -144.5413327229999823 ) ) ;
#5698 = EDGE_CURVE ( 'NONE', #6536, #20642, #7759, .T. ) ;
#5699 = DIRECTION ( 'NONE',  ( -1.000000000000000000, 0.000000000000000000, 0.000000000000000000 ) ) ;
#5700 = CIRCLE ( 'NONE', #9102, 4.000000000000001776 ) ;
#5701 = CIRCLE ( 'NONE', #4944, 2.500000000000000444 ) ;
#5702 = CARTESIAN_POINT ( 'NONE',  ( 18.18320006080000084, -3.000000000000000000, -148.5552959529999839 ) ) ;
#5703 = CARTESIAN_POINT ( 'NONE',  ( -35.47299999999999898, 11.04196010839999964, -144.5552959529999839 ) ) ;
#5704 = DIRECTION ( 'NONE',  ( 1.000000000000000000, 0.000000000000000000, -8.955534726494208689E-12 ) ) ;
#5705 = AXIS2_PLACEMENT_3D ( 'NONE', #14214, #19684, #1623 ) ;
#5706 = CARTESIAN_POINT ( 'NONE',  ( -12.76385253890000016, 37.02886902030000016, -147.6186336929999925 ) ) ;
#5707 = CARTESIAN_POINT ( 'NONE',  ( -20.48150773484949028, 41.30355579012158529, -141.6474779220080222 ) ) ;
#5708 = VERTEX_POINT ( 'NONE', #22639 ) ;
#5709 = CARTESIAN_POINT ( 'NONE',  ( -31.00000000000000000, -50.00000000000000000, -150.0552959529999839 ) ) ;
#5710 = CARTESIAN_POINT ( 'NONE',  ( -6.599319970649999867, -19.98386714700000155, -145.5552959529999839 ) ) ;
#5711 = CARTESIAN_POINT ( 'NONE',  ( 7.500000000000000000, -3.500000000000000000, -150.0552959529999839 ) ) ;
#5712 = LINE ( 'NONE', #2159, #7678 ) ;
#5713 = CARTESIAN_POINT ( 'NONE',  ( -3.499999999959999997, 42.50000000000000000, -136.0552959530000123 ) ) ;
#5714 = ORIENTED_EDGE ( 'NONE', *, *, #710, .F. ) ;
#5715 = CARTESIAN_POINT ( 'NONE',  ( -10.00000000000000000, 48.50000000000000000, -150.0552959529999839 ) ) ;
#5716 = DIRECTION ( 'NONE',  ( 1.000000000000000000, 0.000000000000000000, 0.000000000000000000 ) ) ;
#5717 = ORIENTED_EDGE ( 'NONE', *, *, #8802, .F. ) ;
#5718 = VECTOR ( 'NONE', #6968, 1000.000000000000000 ) ;
#5719 = PRESENTATION_LAYER_ASSIGNMENT (  '', '', ( #6857 ) ) ;
#5720 = EDGE_CURVE ( 'NONE', #19082, #15679, #20738, .T. ) ;
#5721 = ORIENTED_EDGE ( 'NONE', *, *, #11582, .F. ) ;
#5722 = LINE ( 'NONE', #11180, #259 ) ;
#5723 = CARTESIAN_POINT ( 'NONE',  ( -29.45815224832645640, 36.94793816026548683, -140.4653836173310424 ) ) ;
#5724 = CARTESIAN_POINT ( 'NONE',  ( 31.00000000000000000, -0.7500000000009999779, -149.5552959529999839 ) ) ;
#5725 = CARTESIAN_POINT ( 'NONE',  ( 7.908363834111431068, 35.62159694921923858, -141.9696471534852549 ) ) ;
#5726 = ORIENTED_EDGE ( 'NONE', *, *, #5300, .F. ) ;
#5727 = DIRECTION ( 'NONE',  ( 4.511946372079999833E-12, -1.350031197940000176E-13, 1.000000000000000000 ) ) ;
#5728 = EDGE_CURVE ( 'NONE', #22607, #10073, #22287, .T. ) ;
#5729 = CARTESIAN_POINT ( 'NONE',  ( -18.98529451538199808, 32.25804622538513655, -144.7693189751299485 ) ) ;
#5730 = DIRECTION ( 'NONE',  ( 2.507771768020000122E-12, 0.000000000000000000, -1.000000000000000000 ) ) ;
#5731 = FACE_BOUND ( 'NONE', #2168, .T. ) ;
#5732 = CARTESIAN_POINT ( 'NONE',  ( -24.42831371752963676, 38.94399743566808070, -148.4797511750901720 ) ) ;
#5733 = AXIS2_PLACEMENT_3D ( 'NONE', #21744, #16261, #5432 ) ;
#5734 = AXIS2_PLACEMENT_3D ( 'NONE', #10657, #23059, #13894 ) ;
#5735 = CARTESIAN_POINT ( 'NONE',  ( 9.882979739358319193, -19.88614550847407259, -148.5552959529999839 ) ) ;
#5736 = EDGE_CURVE ( 'NONE', #1194, #11089, #18726, .T. ) ;
#5737 = CARTESIAN_POINT ( 'NONE',  ( -20.13043194029999938, 34.25277599949999541, -140.5881547479999938 ) ) ;
#5738 = FACE_OUTER_BOUND ( 'NONE', #17518, .T. ) ;
#5739 = CARTESIAN_POINT ( 'NONE',  ( 19.77963439019999825, -51.26338628519999929, -142.8052959529999839 ) ) ;
#5740 = ORIENTED_EDGE ( 'NONE', *, *, #1259, .T. ) ;
#5741 = CARTESIAN_POINT ( 'NONE',  ( -6.321504075339339224, 40.89356757824499766, -143.5328527138602794 ) ) ;
#5742 = VERTEX_POINT ( 'NONE', #11669 ) ;
#5743 = DIRECTION ( 'NONE',  ( 0.000000000000000000, -1.000000000000000000, 0.000000000000000000 ) ) ;
#5744 = ADVANCED_FACE ( 'NONE', ( #11553 ), #2435, .T. ) ;
#5745 = EDGE_CURVE ( 'NONE', #6134, #21292, #22407, .T. ) ;
#5746 = FACE_OUTER_BOUND ( 'NONE', #1088, .T. ) ;
#5747 = VECTOR ( 'NONE', #22191, 1000.000000000000000 ) ;
#5748 = DIRECTION ( 'NONE',  ( 0.000000000000000000, 1.000000000000000000, 0.000000000000000000 ) ) ;
#5749 = VERTEX_POINT ( 'NONE', #15272 ) ;
#5750 = VECTOR ( 'NONE', #12725, 1000.000000000000000 ) ;
#5751 = CARTESIAN_POINT ( 'NONE',  ( -13.38862532799084804, 35.13131036095179383, -139.8726686351679689 ) ) ;
#5752 = EDGE_CURVE ( 'NONE', #10168, #13979, #2778, .T. ) ;
#5753 = CARTESIAN_POINT ( 'NONE',  ( -15.00000000000000000, -43.00000000000000000, -136.0552959530000123 ) ) ;
#5754 = EDGE_CURVE ( 'NONE', #12827, #20361, #5130, .T. ) ;
#5755 = CARTESIAN_POINT ( 'NONE',  ( 12.50006728695150926, 36.10251055745180082, -150.0552959529999839 ) ) ;
#5756 = DIRECTION ( 'NONE',  ( 0.000000000000000000, -1.000000000000000000, 0.000000000000000000 ) ) ;
#5757 = CARTESIAN_POINT ( 'NONE',  ( -3.500000000000000000, 44.50000000000000000, -151.0552959529999839 ) ) ;
#5758 = DIRECTION ( 'NONE',  ( 0.1146332952500066227, 0.9934078757590583120, 9.947598300640582187E-14 ) ) ;
#5759 = EDGE_LOOP ( 'NONE', ( #2474, #18937, #14357, #11505 ) ) ;
#5760 = DIRECTION ( 'NONE',  ( 1.000000000000000000, 2.602084704489999637E-17, -1.701177084980000217E-20 ) ) ;
#5761 = EDGE_LOOP ( 'NONE', ( #15101, #4676, #431, #2094 ) ) ;
#5762 = ORIENTED_EDGE ( 'NONE', *, *, #19207, .T. ) ;
#5763 = FACE_OUTER_BOUND ( 'NONE', #18255, .T. ) ;
#5764 = CARTESIAN_POINT ( 'NONE',  ( -9.611837139799998653, 32.98927337829999829, -146.0840312179999785 ) ) ;
#5765 = PRESENTATION_LAYER_ASSIGNMENT (  '', '', ( #21752 ) ) ;
#5766 = CIRCLE ( 'NONE', #8796, 2.000000000000001776 ) ;
#5767 = LINE ( 'NONE', #14343, #9255 ) ;
#5768 = AXIS2_PLACEMENT_3D ( 'NONE', #9290, #2073, #23364 ) ;
#5769 = VERTEX_POINT ( 'NONE', #3130 ) ;
#5770 = DIRECTION ( 'NONE',  ( 0.000000000000000000, -1.000000000000000000, 0.000000000000000000 ) ) ;
#5771 = CARTESIAN_POINT ( 'NONE',  ( -30.97299999999999898, 14.00000000000000000, -144.0552959529999839 ) ) ;
#5772 = CARTESIAN_POINT ( 'NONE',  ( -15.00000000000000000, -43.00000000000000000, -136.0552959530000123 ) ) ;
#5773 = VERTEX_POINT ( 'NONE', #21449 ) ;
#5774 = CARTESIAN_POINT ( 'NONE',  ( -20.92079889867846276, 39.38003206206091278, -140.7371765277328279 ) ) ;
#5775 = CARTESIAN_POINT ( 'NONE',  ( 8.822124130990804503, 38.46505108584880617, -142.0295714736415107 ) ) ;
#5776 = ADVANCED_FACE ( 'NONE', ( #23344 ), #23229, .T. ) ;
#5777 = DIRECTION ( 'NONE',  ( -1.000000000000000000, 0.000000000000000000, 2.257157423930000049E-12 ) ) ;
#5778 = PLANE ( 'NONE',  #5199 ) ;
#5779 =( GEOMETRIC_REPRESENTATION_CONTEXT ( 3 ) GLOBAL_UNCERTAINTY_ASSIGNED_CONTEXT ( ( #2495 ) ) GLOBAL_UNIT_ASSIGNED_CONTEXT ( ( #9901, #13480, #647 ) ) REPRESENTATION_CONTEXT ( 'NONE', 'WORKASPACE' ) );
#5780 = ORIENTED_EDGE ( 'NONE', *, *, #10942, .T. ) ;
#5781 = AXIS2_PLACEMENT_3D ( 'NONE', #19116, #15544, #2819 ) ;
#5782 = LINE ( 'NONE', #13041, #7269 ) ;
#5783 = EDGE_LOOP ( 'NONE', ( #21758, #22903, #22426, #6984 ) ) ;
#5784 = PRESENTATION_STYLE_ASSIGNMENT (( #3776 ) ) ;
#5785 = ORIENTED_EDGE ( 'NONE', *, *, #12393, .F. ) ;
#5786 = CARTESIAN_POINT ( 'NONE',  ( -26.38328323801417241, 40.40271240115249896, -146.0760205945481118 ) ) ;
#5787 = ORIENTED_EDGE ( 'NONE', *, *, #9768, .F. ) ;
#5788 = DIRECTION ( 'NONE',  ( 0.000000000000000000, -1.000000000000000000, 0.000000000000000000 ) ) ;
#5789 = ORIENTED_EDGE ( 'NONE', *, *, #13313, .T. ) ;
#5790 = CARTESIAN_POINT ( 'NONE',  ( -34.35824191590000254, -1.500000000000000000, -150.0657682190000060 ) ) ;
#5791 = ORIENTED_EDGE ( 'NONE', *, *, #11985, .T. ) ;
#5792 = SHAPE_DEFINITION_REPRESENTATION ( #11883, #538 ) ;
#5793 = ORIENTED_EDGE ( 'NONE', *, *, #6622, .F. ) ;
#5794 = CARTESIAN_POINT ( 'NONE',  ( -27.96130559120596715, 37.85361357870127108, -147.7859560200423061 ) ) ;
#5795 = CARTESIAN_POINT ( 'NONE',  ( -14.40511015810000117, 39.11695720679999511, -141.1121292869999877 ) ) ;
#5796 = DIRECTION ( 'NONE',  ( 2.257749542879999954E-12, 0.000000000000000000, 1.000000000000000000 ) ) ;
#5797 = PRESENTATION_LAYER_ASSIGNMENT (  '', '', ( #13017 ) ) ;
#5798 = LINE ( 'NONE', #11371, #14768 ) ;
#5799 = AXIS2_PLACEMENT_3D ( 'NONE', #631, #15019, #15263 ) ;
#5800 = CARTESIAN_POINT ( 'NONE',  ( -6.766664769653541356, 35.09179379324020687, -148.4985462000928180 ) ) ;
#5801 = EDGE_CURVE ( 'NONE', #10478, #9593, #6922, .T. ) ;
#5802 = CARTESIAN_POINT ( 'NONE',  ( -2.499999999959999997, 40.00000000000000000, -153.0552959529999839 ) ) ;
#5803 = ORIENTED_EDGE ( 'NONE', *, *, #1770, .T. ) ;
#5804 = DIRECTION ( 'NONE',  ( 0.000000000000000000, -1.000000000000000000, 0.000000000000000000 ) ) ;
#5805 = CARTESIAN_POINT ( 'NONE',  ( 19.13369214859999801, 50.50000000000000000, -136.0552959530000123 ) ) ;
#5806 = VERTEX_POINT ( 'NONE', #17876 ) ;
#5807 = DIRECTION ( 'NONE',  ( 0.000000000000000000, 2.256988247090000272E-12, 1.000000000000000000 ) ) ;
#5809 = CARTESIAN_POINT ( 'NONE',  ( -12.67903993044300215, 40.83408799367548880, -146.3170871812478708 ) ) ;
#5808 = ADVANCED_BREP_SHAPE_REPRESENTATION ( '', ( #19584, #5025 ), #3536 ) ;
#5810 = PLANE ( 'NONE',  #10912 ) ;
#5811 = CARTESIAN_POINT ( 'NONE',  ( -29.40140556760018953, 40.21055626237175318, -145.9944493861516435 ) ) ;
#5812 = ORIENTED_EDGE ( 'NONE', *, *, #13240, .T. ) ;
#5813 = CARTESIAN_POINT ( 'NONE',  ( -32.50000000000000000, -36.00000000000000000, -150.0552959529999839 ) ) ;
#5814 =( GEOMETRIC_REPRESENTATION_CONTEXT ( 3 ) GLOBAL_UNCERTAINTY_ASSIGNED_CONTEXT ( ( #3747 ) ) GLOBAL_UNIT_ASSIGNED_CONTEXT ( ( #1198, #4862, #21176 ) ) REPRESENTATION_CONTEXT ( 'NONE', 'WORKASPACE' ) );
#5815 = DIRECTION ( 'NONE',  ( -1.000000000000000000, 0.000000000000000000, 0.000000000000000000 ) ) ;
#5816 = ORIENTED_EDGE ( 'NONE', *, *, #16653, .T. ) ;
#5817 = CARTESIAN_POINT ( 'NONE',  ( 15.50000000000000000, 33.50000000000000000, -137.0552959530000123 ) ) ;
#5818 = CARTESIAN_POINT ( 'NONE',  ( 18.95053822279999878, -50.00000000000000000, -149.5552959529999839 ) ) ;
#5819 = DIRECTION ( 'NONE',  ( 0.9996028016287901163, -0.02818224575639410520, -1.295785648389728035E-13 ) ) ;
#5820 = CARTESIAN_POINT ( 'NONE',  ( -20.28536656038299668, 36.96856293253134851, -139.5160734783616476 ) ) ;
#5821 = EDGE_LOOP ( 'NONE', ( #2727, #13598, #7084, #6987 ) ) ;
#5822 = CARTESIAN_POINT ( 'NONE',  ( -27.11867290101617556, 36.95185637389150912, -147.5185143933871075 ) ) ;
#5823 = CARTESIAN_POINT ( 'NONE',  ( 19.77963439019999825, -51.26338628519999929, -142.8052959529999839 ) ) ;
#5824 = DIRECTION ( 'NONE',  ( -2.842170943040000002E-14, -3.552713678800000097E-13, -1.000000000000000000 ) ) ;
#5825 = CYLINDRICAL_SURFACE ( 'NONE', #18334, 0.7500000000000016653 ) ;
#5826 = CARTESIAN_POINT ( 'NONE',  ( -4.726769794276915349, 42.89852487308498752, -136.0552959529893258 ) ) ;
#5827 = EDGE_LOOP ( 'NONE', ( #21279, #446, #276, #12698 ) ) ;
#5828 = EDGE_CURVE ( 'NONE', #404, #19705, #18587, .T. ) ;
#5829 = DIRECTION ( 'NONE',  ( 1.000000000000000000, 0.000000000000000000, -8.954760363766765626E-12 ) ) ;
#5830 = CARTESIAN_POINT ( 'NONE',  ( -15.00000000000000000, -44.50000000000000000, -136.0552959530000123 ) ) ;
#5831 = ADVANCED_FACE ( 'NONE', ( #15620 ), #6800, .F. ) ;
#5832 = ORIENTED_EDGE ( 'NONE', *, *, #23057, .F. ) ;
#5833 = AXIS2_PLACEMENT_3D ( 'NONE', #18620, #16835, #2336 ) ;
#5834 = APPLICATION_CONTEXT ( 'automotive_design' ) ;
#5835 = ORIENTED_EDGE ( 'NONE', *, *, #13313, .F. ) ;
#5836 = CARTESIAN_POINT ( 'NONE',  ( -22.48976697757457544, 37.06353063726731278, -140.4055699430355730 ) ) ;
#5837 = CARTESIAN_POINT ( 'NONE',  ( 32.50000000000000000, -33.03620104880000241, -136.0552959530000123 ) ) ;
#5838 = CARTESIAN_POINT ( 'NONE',  ( -21.83347610789999749, 32.92361448670000357, -143.4947777360000032 ) ) ;
#5839 = CARTESIAN_POINT ( 'NONE',  ( 7.662331531295155429, 35.75568826264862565, -141.8869580487122732 ) ) ;
#5840 = ORIENTED_EDGE ( 'NONE', *, *, #17681, .T. ) ;
#5841 = LINE ( 'NONE', #14894, #10134 ) ;
#5842 = DIRECTION ( 'NONE',  ( 5.228780262857720083E-12, 0.000000000000000000, 1.000000000000000000 ) ) ;
#5843 = FACE_OUTER_BOUND ( 'NONE', #22466, .T. ) ;
#5844 = FACE_OUTER_BOUND ( 'NONE', #5761, .T. ) ;
#5845 = CARTESIAN_POINT ( 'NONE',  ( -23.96729089091851961, 37.81249143152112424, -148.2640374881100058 ) ) ;
#5846 = CARTESIAN_POINT ( 'NONE',  ( -16.48779918059999616, 32.42295671489999620, -143.3618442240000093 ) ) ;
#5847 = VECTOR ( 'NONE', #1340, 1000.000000000000000 ) ;
#5848 = PLANE ( 'NONE',  #8797 ) ;
#5849 = CARTESIAN_POINT ( 'NONE',  ( -21.71608528419999828, -34.50000000000000000, -144.8157682190000060 ) ) ;
#5850 = LINE ( 'NONE', #6212, #10778 ) ;
#5851 = ORIENTED_EDGE ( 'NONE', *, *, #23496, .F. ) ;
#5852 = B_SPLINE_CURVE_WITH_KNOTS ( 'NONE', 3,
 ( #21931, #16799, #22270, #7627, #14779, #16560, #268, #14900, #22158, #13215, #20490, #4191, #11425, #6203, #10346, #10105, #1094, #22733 ),
 .UNSPECIFIED., .F., .F.,
 ( 4, 2, 2, 2, 2, 2, 2, 2, 4 ),
 ( 0.000000000000000000, 0.1250000000000000000, 0.2500000000000000000, 0.3750000000000000000, 0.5000000000000000000, 0.6250000000000000000, 0.7500000000000000000, 0.8750000000000000000, 1.000000000000000000 ),
 .UNSPECIFIED. ) ;
#5853 = CARTESIAN_POINT ( 'NONE',  ( -5.199058631898605398, 40.19233567625393988, -142.2195710326207347 ) ) ;
#5854 = CARTESIAN_POINT ( 'NONE',  ( 1.342750202250000191, -63.28208324180000233, -144.5552959529999839 ) ) ;
#5855 = ADVANCED_FACE ( 'NONE', ( #16088 ), #5249, .T. ) ;
#5856 = ORIENTED_EDGE ( 'NONE', *, *, #10165, .T. ) ;
#5857 = CARTESIAN_POINT ( 'NONE',  ( -31.00000000000000000, -7.105427357599999217E-15, -149.5552959529999839 ) ) ;
#5858 = CARTESIAN_POINT ( 'NONE',  ( 5.578707461739999651, -1.525439235750000178, -135.5552959530000123 ) ) ;
#5859 = DIRECTION ( 'NONE',  ( 1.000000000000000000, 0.000000000000000000, -4.510281037539696830E-12 ) ) ;
#5860 = EDGE_LOOP ( 'NONE', ( #11363, #3982, #1789, #16154 ) ) ;
#5861 = CARTESIAN_POINT ( 'NONE',  ( -13.01778940292994946, 33.53025516020306185, -144.5305955197007393 ) ) ;
#5862 = LINE ( 'NONE', #17168, #5919 ) ;
#5863 = VECTOR ( 'NONE', #21326, 1000.000000000000000 ) ;
#5864 = EDGE_CURVE ( 'NONE', #8505, #21499, #14069, .T. ) ;
#5865 = DIRECTION ( 'NONE',  ( 1.000000000000000000, 0.000000000000000000, 2.516505522483685870E-12 ) ) ;
#5866 = CYLINDRICAL_SURFACE ( 'NONE', #7498, 2.000000000000000000 ) ;
#5867 = DIRECTION ( 'NONE',  ( 0.000000000000000000, 1.000000000000000000, 0.000000000000000000 ) ) ;
#5868 = CARTESIAN_POINT ( 'NONE',  ( 4.332174032634473093, -37.80157851245341760, -150.0552959529999555 ) ) ;
#5869 = ORIENTED_EDGE ( 'NONE', *, *, #9089, .F. ) ;
#5870 = CARTESIAN_POINT ( 'NONE',  ( -28.18164916495271655, 37.07873981898632110, -148.1638686014701989 ) ) ;
#5871 = ORIENTED_EDGE ( 'NONE', *, *, #16910, .F. ) ;
#5872 =( NAMED_UNIT ( * ) SI_UNIT ( $, .STERADIAN. ) SOLID_ANGLE_UNIT ( ) );
#5873 = ADVANCED_FACE ( 'NONE', ( #19782 ), #1346, .F. ) ;
#5874 = EDGE_CURVE ( 'NONE', #16725, #4317, #8348, .T. ) ;
#5875 = EDGE_LOOP ( 'NONE', ( #17390, #14552, #23199, #22850, #17101, #7094, #18541, #6755 ) ) ;
#5876 = CARTESIAN_POINT ( 'NONE',  ( -13.75718804428722741, 33.24050247982404471, -144.6561462772629056 ) ) ;
#5877 = CARTESIAN_POINT ( 'NONE',  ( -10.46662683120000104, 35.31824366040000029, -139.9138328150000063 ) ) ;
#5878 = DIRECTION ( 'NONE',  ( 0.000000000000000000, 0.000000000000000000, 1.000000000000000000 ) ) ;
#5879 = ADVANCED_FACE ( 'NONE', ( #8465 ), #10362, .T. ) ;
#5880 = ORIENTED_EDGE ( 'NONE', *, *, #7675, .T. ) ;
#5881 = DIRECTION ( 'NONE',  ( 0.000000000000000000, 0.000000000000000000, 1.000000000000000000 ) ) ;
#5882 = EDGE_CURVE ( 'NONE', #7389, #7704, #6570, .T. ) ;
#5883 = DIRECTION ( 'NONE',  ( -5.094701932209999624E-24, -1.000000000000000000, 1.149947916579999802E-35 ) ) ;
#5884 = VECTOR ( 'NONE', #15466, 1000.000000000000000 ) ;
#5885 = ORIENTED_EDGE ( 'NONE', *, *, #19180, .F. ) ;
#5886 = CARTESIAN_POINT ( 'NONE',  ( -21.59845619502680591, 40.49633916123557498, -146.0585726302816454 ) ) ;
#5887 = CARTESIAN_POINT ( 'NONE',  ( 9.767209682567662199, 37.80278906969247288, -141.6876531319532546 ) ) ;
#5888 = CARTESIAN_POINT ( 'NONE',  ( -34.50000000000000000, 67.50000000000000000, -144.0552959529999839 ) ) ;
#5889 = EDGE_CURVE ( 'NONE', #213, #3522, #13834, .T. ) ;
#5890 = FACE_OUTER_BOUND ( 'NONE', #5247, .T. ) ;
#5891 = ADVANCED_FACE ( 'NONE', ( #4790 ), #12033, .F. ) ;
#5892 = ORIENTED_EDGE ( 'NONE', *, *, #15345, .F. ) ;
#5893 = DIRECTION ( 'NONE',  ( 2.257171095940000041E-12, 1.003664318210000046E-28, 1.000000000000000000 ) ) ;
#5894 = VERTEX_POINT ( 'NONE', #6681 ) ;
#5895 = VECTOR ( 'NONE', #10342, 1000.000000000000000 ) ;
#5896 =( NAMED_UNIT ( * ) SI_UNIT ( $, .STERADIAN. ) SOLID_ANGLE_UNIT ( ) );
#5897 = VECTOR ( 'NONE', #9104, 1000.000000000000000 ) ;
#5898 = VERTEX_POINT ( 'NONE', #4905 ) ;
#5899 = CARTESIAN_POINT ( 'NONE',  ( -26.50527565058495938, 41.51083911114544378, -144.5405030844974021 ) ) ;
#5900 = ADVANCED_FACE ( 'NONE', ( #19425 ), #5026, .T. ) ;
#5901 = EDGE_LOOP ( 'NONE', ( #14706, #6579, #1130, #193 ) ) ;
#5902 = DIRECTION ( 'NONE',  ( 0.7071067811866730279, 0.3390050494208429743, 0.6205445805637129775 ) ) ;
#5903 = EDGE_CURVE ( 'NONE', #17995, #16183, #6287, .T. ) ;
#5904 = ORIENTED_EDGE ( 'NONE', *, *, #11945, .F. ) ;
#5905 = DIRECTION ( 'NONE',  ( 0.000000000000000000, -1.000000000000000000, 0.000000000000000000 ) ) ;
#5906 = ORIENTED_EDGE ( 'NONE', *, *, #11985, .F. ) ;
#5907 = CARTESIAN_POINT ( 'NONE',  ( 0.000000000000000000, 0.000000000000000000, 0.000000000000000000 ) ) ;
#5908 = ADVANCED_FACE ( 'NONE', ( #7277 ), #12626, .T. ) ;
#5909 = VERTEX_POINT ( 'NONE', #13174 ) ;
#5910 = CARTESIAN_POINT ( 'NONE',  ( -27.79745750754647560, 38.94545112596043879, -148.2735626928909483 ) ) ;
#5911 = CARTESIAN_POINT ( 'NONE',  ( 16.82730212879999598, -31.88969284570000084, -146.0552959529999839 ) ) ;
#5912 = LINE ( 'NONE', #13167, #21379 ) ;
#5913 = CARTESIAN_POINT ( 'NONE',  ( 0.5000000001409999895, 24.10555127549999810, -147.5552959529999839 ) ) ;
#5914 = CARTESIAN_POINT ( 'NONE',  ( -6.131111726649999483, 36.14321585209999910, -147.9535578170000178 ) ) ;
#5915 = CARTESIAN_POINT ( 'NONE',  ( -7.828824709450000086, 39.51093879980000168, -140.6700787229999889 ) ) ;
#5916 = ORIENTED_EDGE ( 'NONE', *, *, #470, .T. ) ;
#5917 = FACE_OUTER_BOUND ( 'NONE', #10664, .T. ) ;
#5918 = VECTOR ( 'NONE', #11272, 1000.000000000000000 ) ;
#5919 = VECTOR ( 'NONE', #16930, 1000.000000000000000 ) ;
#5920 = DIRECTION ( 'NONE',  ( 0.000000000000000000, 1.000000000000000000, 2.245315043809999812E-12 ) ) ;
#5921 = LINE ( 'NONE', #20448, #12498 ) ;
#5922 = ORIENTED_EDGE ( 'NONE', *, *, #16952, .T. ) ;
#5923 = CARTESIAN_POINT ( 'NONE',  ( -12.94305406498005162, 37.05025962682652363, -148.5780888799759794 ) ) ;
#5924 = CARTESIAN_POINT ( 'NONE',  ( -18.39977846769595615, 38.96581140717537295, -148.3858654058074080 ) ) ;
#5925 = CARTESIAN_POINT ( 'NONE',  ( -22.00705883600000234, 37.05789963359999462, -148.1619053240000028 ) ) ;
#5926 = ORIENTED_EDGE ( 'NONE', *, *, #13843, .F. ) ;
#5927 = CARTESIAN_POINT ( 'NONE',  ( -7.499999999959999997, 25.50000000000000000, -136.0552959530000123 ) ) ;
#5928 = LINE ( 'NONE', #22473, #615 ) ;
#5929 = ORIENTED_EDGE ( 'NONE', *, *, #22327, .F. ) ;
#5930 = DIRECTION ( 'NONE',  ( 0.000000000000000000, 0.000000000000000000, -1.000000000000000000 ) ) ;
#5931 = DIRECTION ( 'NONE',  ( 1.000000000000000000, 0.000000000000000000, -2.257171095940000041E-12 ) ) ;
#5932 = EDGE_CURVE ( 'NONE', #546, #8661, #20563, .T. ) ;
#5933 = ORIENTED_EDGE ( 'NONE', *, *, #10246, .T. ) ;
#5934 = DIRECTION ( 'NONE',  ( 3.494344380199214996E-12, 0.000000000000000000, -1.000000000000000000 ) ) ;
#5935 = EDGE_CURVE ( 'NONE', #9692, #10310, #9707, .T. ) ;
#5936 = VECTOR ( 'NONE', #21126, 1000.000000000000000 ) ;
#5937 = CARTESIAN_POINT ( 'NONE',  ( -21.31949744912997957, 39.81204609393142846, -147.9708906465881455 ) ) ;
#5938 = VECTOR ( 'NONE', #4824, 1000.000000000000000 ) ;
#5939 = ORIENTED_EDGE ( 'NONE', *, *, #21313, .T. ) ;
#5940 = CARTESIAN_POINT ( 'NONE',  ( -27.77832206610000298, 37.03059619289999915, -147.6270870419999710 ) ) ;
#5941 = DIRECTION ( 'NONE',  ( -2.510584333019999972E-12, 0.000000000000000000, 1.000000000000000000 ) ) ;
#5942 = ORIENTED_EDGE ( 'NONE', *, *, #21036, .T. ) ;
#5943 = DIRECTION ( 'NONE',  ( -1.000000000000000000, 0.000000000000000000, 2.245315044999999693E-12 ) ) ;
#5944 = CARTESIAN_POINT ( 'NONE',  ( -33.50000000000000000, 26.00000000000000000, -137.5552959530000123 ) ) ;
#5945 = DIRECTION ( 'NONE',  ( 1.000000000000000000, 0.000000000000000000, -2.715621035259064790E-14 ) ) ;
#5946 = ORIENTED_EDGE ( 'NONE', *, *, #19571, .T. ) ;
#5947 = FACE_BOUND ( 'NONE', #17091, .T. ) ;
#5948 = CARTESIAN_POINT ( 'NONE',  ( -3.499999999959999997, 46.50000000000000000, -136.0552959530000123 ) ) ;
#5949 = ORIENTED_EDGE ( 'NONE', *, *, #14618, .F. ) ;
#5950 = VERTEX_POINT ( 'NONE', #11496 ) ;
#5951 = CARTESIAN_POINT ( 'NONE',  ( -23.38637323487361286, 36.19895251858893204, -140.4460590724356450 ) ) ;
#5952 = CARTESIAN_POINT ( 'NONE',  ( -30.26175564716108823, 41.48858102658289226, -145.0104668248091286 ) ) ;
#5953 = DIRECTION ( 'NONE',  ( 4.430318231639999944E-12, -6.100259101500000139E-13, 1.000000000000000000 ) ) ;
#5954 = CARTESIAN_POINT ( 'NONE',  ( 8.500000000060001781, 35.50000000000000000, -142.0552959529999839 ) ) ;
#5955 = ORIENTED_EDGE ( 'NONE', *, *, #6555, .T. ) ;
#5956 = DIRECTION ( 'NONE',  ( 1.000000000000000000, 0.000000000000000000, 0.000000000000000000 ) ) ;
#5957 = EDGE_CURVE ( 'NONE', #7225, #14794, #5921, .T. ) ;
#5958 = EDGE_CURVE ( 'NONE', #22397, #18180, #8707, .T. ) ;
#5959 = DIRECTION ( 'NONE',  ( 1.000000000000000000, 0.000000000000000000, -4.511206223393553012E-12 ) ) ;
#5960 = CARTESIAN_POINT ( 'NONE',  ( -9.389499115566652065, 36.98418387195368950, -147.3811924092332788 ) ) ;
#5961 = EDGE_CURVE ( 'NONE', #1387, #13267, #11295, .T. ) ;
#5962 = CARTESIAN_POINT ( 'NONE',  ( -24.08804847542923255, 41.25040067026291979, -146.5677998250044425 ) ) ;
#5963 = EDGE_CURVE ( 'NONE', #8780, #19806, #14969, .T. ) ;
#5964 = CARTESIAN_POINT ( 'NONE',  ( -15.35382742459208494, 35.97464847315127656, -148.5826496918325859 ) ) ;
#5965 = VECTOR ( 'NONE', #18837, 1000.000000000000000 ) ;
#5966 = CARTESIAN_POINT ( 'NONE',  ( -17.23374593961228740, 34.42700048754028330, -140.4054235586860955 ) ) ;
#5967 = MECHANICAL_DESIGN_GEOMETRIC_PRESENTATION_REPRESENTATION (  '', ( #8996 ), #23098 ) ;
#5968 = PLANE ( 'NONE',  #9926 ) ;
#5969 = FACE_OUTER_BOUND ( 'NONE', #16544, .T. ) ;
#5970 = DIRECTION ( 'NONE',  ( 0.4437127003902655575, 0.8961690909155359819, -7.993605777301127091E-13 ) ) ;
#5971 = ORIENTED_EDGE ( 'NONE', *, *, #21770, .T. ) ;
#5972 = CARTESIAN_POINT ( 'NONE',  ( -5.673950476189068226, 38.39705415069988703, -140.7335603934562585 ) ) ;
#5973 = FACE_BOUND ( 'NONE', #1281, .T. ) ;
#5974 = EDGE_LOOP ( 'NONE', ( #15184, #2605, #17443, #16857 ) ) ;
#5975 = CARTESIAN_POINT ( 'NONE',  ( 2.016283561950000358, -13.16498300129999954, -143.0552959529999839 ) ) ;
#5976 = LINE ( 'NONE', #6103, #11346 ) ;
#5977 = VERTEX_POINT ( 'NONE', #19897 ) ;
#5978 = CARTESIAN_POINT ( 'NONE',  ( -12.18657821949179798, 35.21158449346761898, -148.0902736314953643 ) ) ;
#5979 = CIRCLE ( 'NONE', #11285, 2.000000000000001776 ) ;
#5980 = LINE ( 'NONE', #998, #1383 ) ;
#5981 = AXIS2_PLACEMENT_3D ( 'NONE', #12718, #17971, #6896 ) ;
#5982 = CARTESIAN_POINT ( 'NONE',  ( 3.999999999879999546, -1.500000000000000000, -135.2552959529999725 ) ) ;
#5983 = CARTESIAN_POINT ( 'NONE',  ( -27.49486172903680981, 36.99676060752976525, -147.4549925864818363 ) ) ;
#5984 = DIRECTION ( 'NONE',  ( -1.000000000000000000, 0.000000000000000000, 0.000000000000000000 ) ) ;
#5985 = DIRECTION ( 'NONE',  ( -1.000000000000000000, 0.000000000000000000, 2.257144641399999941E-12 ) ) ;
#5986 = ORIENTED_EDGE ( 'NONE', *, *, #368, .T. ) ;
#5987 = EDGE_CURVE ( 'NONE', #6638, #8120, #4371, .T. ) ;
#5988 = CARTESIAN_POINT ( 'NONE',  ( -28.72801644006947797, 33.22604713767264428, -144.4610326614979954 ) ) ;
#5989 = ORIENTED_EDGE ( 'NONE', *, *, #437, .T. ) ;
#5990 = SURFACE_SIDE_STYLE ('',( #2331 ) ) ;
#5991 = ORIENTED_EDGE ( 'NONE', *, *, #19570, .T. ) ;
#5992 = CARTESIAN_POINT ( 'NONE',  ( -6.389646268539595830, 36.98420143703149421, -147.3954793909555008 ) ) ;
#5993 = DIRECTION ( 'NONE',  ( 0.000000000000000000, 1.000000000000000000, 0.000000000000000000 ) ) ;
#5994 = CARTESIAN_POINT ( 'NONE',  ( -9.373415772411227920, -17.59966358942910958, -143.5552959529999839 ) ) ;
#5996 = AXIS2_PLACEMENT_3D ( 'NONE', #9870, #17144, #866 ) ;
#5995 = PRODUCT_RELATED_PRODUCT_CATEGORY ( 'part', '', ( #4218 ) ) ;
#5997 = ORIENTED_EDGE ( 'NONE', *, *, #3334, .T. ) ;
#5998 = CARTESIAN_POINT ( 'NONE',  ( 7.750000000000000000, -42.23606797749999942, -151.0552959529999839 ) ) ;
#5999 = EDGE_CURVE ( 'NONE', #14365, #3115, #15174, .T. ) ;
#6000 = DIRECTION ( 'NONE',  ( 5.094701932209999624E-24, 1.000000000000000000, -1.149947916579999802E-35 ) ) ;
#6001 = AXIS2_PLACEMENT_3D ( 'NONE', #19607, #15797, #14251 ) ;
#6002 = VERTEX_POINT ( 'NONE', #17994 ) ;
#6003 = CARTESIAN_POINT ( 'NONE',  ( -20.36280570450795935, 40.92149091605320166, -144.5882336176783838 ) ) ;
#6004 = CARTESIAN_POINT ( 'NONE',  ( 9.606946132914400138, 38.01234624700477127, -141.7694449706205546 ) ) ;
#6005 =( BOUNDED_CURVE ( )  B_SPLINE_CURVE ( 5, ( #15554, #22463, #2596, #21039, #820, #13408 ),
 .UNSPECIFIED., .F., .F. ) 
 B_SPLINE_CURVE_WITH_KNOTS ( ( 6, 6 ),
 ( 1.570796326821625177, 3.141592653590000062 ),
 .UNSPECIFIED. ) 
 CURVE ( )  GEOMETRIC_REPRESENTATION_ITEM ( )  RATIONAL_B_SPLINE_CURVE ( ( 0.2500000000000000000, 0.2500000000033899550, 0.3000000000050849769, 0.4000000000067799877, 0.6000000000067799988, 1.000000000000000000 ) ) 
 REPRESENTATION_ITEM ( '' )  );
#6006 = ADVANCED_FACE ( 'NONE', ( #11381 ), #7816, .F. ) ;
#6007 = FACE_OUTER_BOUND ( 'NONE', #1883, .T. ) ;
#6008 = LINE ( 'NONE', #13261, #16239 ) ;
#6009 = EDGE_LOOP ( 'NONE', ( #2537, #6884, #3824, #21235 ) ) ;
#6010 = VECTOR ( 'NONE', #6795, 1000.000000000000000 ) ;
#6011 = CARTESIAN_POINT ( 'NONE',  ( -32.50000000000000000, -36.00000000000000000, -143.3052959529999839 ) ) ;
#6012 = AXIS2_PLACEMENT_3D ( 'NONE', #13338, #18814, #22271 ) ;
#6013 = ORIENTED_EDGE ( 'NONE', *, *, #6506, .T. ) ;
#6014 = CARTESIAN_POINT ( 'NONE',  ( 6.485119744325247737, -49.00006725843046951, -150.0552959529999839 ) ) ;
#6015 = ADVANCED_FACE ( 'NONE', ( #2377 ), #7153, .F. ) ;
#6016 = EDGE_LOOP ( 'NONE', ( #1645, #22299, #480, #15898 ) ) ;
#6017 = CARTESIAN_POINT ( 'NONE',  ( -26.92260725150358525, 38.41501433962203294, -147.3424669775142206 ) ) ;
#6018 = VERTEX_POINT ( 'NONE', #14544 ) ;
#6019 = AXIS2_PLACEMENT_3D ( 'NONE', #23427, #16173, #18073 ) ;
#6020 = DIRECTION ( 'NONE',  ( 0.000000000000000000, 0.000000000000000000, 1.000000000000000000 ) ) ;
#6021 = ORIENTED_EDGE ( 'NONE', *, *, #12130, .T. ) ;
#6022 = CARTESIAN_POINT ( 'NONE',  ( -11.99999999999999467, -43.39269908169870860, -150.0552959529999555 ) ) ;
#6023 = ORIENTED_EDGE ( 'NONE', *, *, #3107, .T. ) ;
#6024 = ORIENTED_EDGE ( 'NONE', *, *, #16214, .T. ) ;
#6025 = CARTESIAN_POINT ( 'NONE',  ( -26.73151279712584127, 41.02465574057303854, -146.3859699703060073 ) ) ;
#6026 = ADVANCED_FACE ( 'NONE', ( #21809 ), #12740, .T. ) ;
#6027 = CARTESIAN_POINT ( 'NONE',  ( -15.17828643430000035, 39.13746915040000118, -146.9793796819999727 ) ) ;
#6028 = FACE_OUTER_BOUND ( 'NONE', #3244, .T. ) ;
#6029 = EDGE_CURVE ( 'NONE', #1030, #23189, #244, .T. ) ;
#6030 = DIRECTION ( 'NONE',  ( -0.7633862853691523176, -0.6459422414661291079, 0.000000000000000000 ) ) ;
#6031 = CARTESIAN_POINT ( 'NONE',  ( -7.305231917203080627, 34.61982510850948103, -147.5275646996967964 ) ) ;
#6032 = VECTOR ( 'NONE', #10884, 1000.000000000000000 ) ;
#6033 = CARTESIAN_POINT ( 'NONE',  ( -7.955559433785680312, 37.98585944842262307, -139.4072494953622083 ) ) ;
#6034 = ORIENTED_EDGE ( 'NONE', *, *, #1973, .F. ) ;
#6035 = CIRCLE ( 'NONE', #13643, 5.000000000000000000 ) ;
#6036 = CARTESIAN_POINT ( 'NONE',  ( -32.50000000000000000, 26.00000000000000000, -148.5552959529999839 ) ) ;
#6037 = VECTOR ( 'NONE', #6910, 1000.000000000000227 ) ;
#6038 = ADVANCED_FACE ( 'NONE', ( #15790 ), #4846, .F. ) ;
#6039 = CARTESIAN_POINT ( 'NONE',  ( -8.770737564319999180, -11.35481373070000011, -144.5552959529999839 ) ) ;
#6040 = AXIS2_PLACEMENT_3D ( 'NONE', #14127, #13886, #16148 ) ;
#6041 = EDGE_CURVE ( 'NONE', #13199, #21050, #20924, .T. ) ;
#6042 = CARTESIAN_POINT ( 'NONE',  ( 2.500000000170000014, 20.50000000000000000, -136.5552959530000123 ) ) ;
#6043 = ORIENTED_EDGE ( 'NONE', *, *, #7925, .F. ) ;
#6044 = EDGE_CURVE ( 'NONE', #20527, #22590, #8281, .T. ) ;
#6045 = CARTESIAN_POINT ( 'NONE',  ( -12.63886943596979684, 40.45021591189686916, -146.0874523975345483 ) ) ;
#6046 = EDGE_CURVE ( 'NONE', #11453, #1427, #21160, .T. ) ;
#6047 = PLANE ( 'NONE',  #3321 ) ;
#6048 = DIRECTION ( 'NONE',  ( 0.000000000000000000, -1.000000000000000000, 0.000000000000000000 ) ) ;
#6049 = VERTEX_POINT ( 'NONE', #6513 ) ;
#6050 = CARTESIAN_POINT ( 'NONE',  ( 4.500000000009999113, -3.500000000000000000, -137.0552959530000123 ) ) ;
#6051 = CARTESIAN_POINT ( 'NONE',  ( -31.00000000000000000, -7.105427357599999217E-15, -149.5552959529999839 ) ) ;
#6052 = AXIS2_PLACEMENT_3D ( 'NONE', #10943, #21276, #10308 ) ;
#6053 = ORIENTED_EDGE ( 'NONE', *, *, #2936, .F. ) ;
#6054 = CARTESIAN_POINT ( 'NONE',  ( 10.93320006080000084, -15.50000000000000000, -148.5552959529999839 ) ) ;
#6055 = CARTESIAN_POINT ( 'NONE',  ( -30.49999999990000177, 26.50000000000000000, -147.5552959529999839 ) ) ;
#6056 = ORIENTED_EDGE ( 'NONE', *, *, #6974, .T. ) ;
#6057 = DIRECTION ( 'NONE',  ( -1.000000000000000000, 0.000000000000000000, 2.257144641399999941E-12 ) ) ;
#6058 = VECTOR ( 'NONE', #12716, 1000.000000000000000 ) ;
#6059 = CARTESIAN_POINT ( 'NONE',  ( -20.75267599334476643, 38.70207599832220069, -148.1344118532358323 ) ) ;
#6060 = EDGE_LOOP ( 'NONE', ( #10876, #10070, #19071, #1430 ) ) ;
#6061 = SURFACE_SIDE_STYLE ('',( #9497 ) ) ;
#6062 = CARTESIAN_POINT ( 'NONE',  ( -27.75437169045599006, 33.36630509636427178, -144.3381695521194104 ) ) ;
#6063 = VECTOR ( 'NONE', #1869, 1000.000000000000000 ) ;
#6064 = LINE ( 'NONE', #13315, #7981 ) ;
#6065 = ORIENTED_EDGE ( 'NONE', *, *, #13234, .T. ) ;
#6066 = AXIS2_PLACEMENT_3D ( 'NONE', #8056, #6280, #13534 ) ;
#6067 = CARTESIAN_POINT ( 'NONE',  ( 31.50000000000000000, 0.000000000000000000, -150.0552959529999839 ) ) ;
#6068 = CARTESIAN_POINT ( 'NONE',  ( 6.477506801250000557, -13.91317765220000169, -146.5552959529999839 ) ) ;
#6069 = CARTESIAN_POINT ( 'NONE',  ( -4.020805332062283632, 42.55092418646380281, -136.0552959529909458 ) ) ;
#6070 = VERTEX_POINT ( 'NONE', #18886 ) ;
#6071 = PLANE ( 'NONE',  #14780 ) ;
#6072 = DIRECTION ( 'NONE',  ( -1.000000000000000000, 0.000000000000000000, 0.000000000000000000 ) ) ;
#6073 = ORIENTED_EDGE ( 'NONE', *, *, #22277, .T. ) ;
#6074 = ADVANCED_FACE ( 'NONE', ( #13780 ), #2598, .F. ) ;
#6075 = EDGE_LOOP ( 'NONE', ( #23400, #16518, #2161 ) ) ;
#6076 = AXIS2_PLACEMENT_3D ( 'NONE', #6705, #4695, #5052 ) ;
#6077 = AXIS2_PLACEMENT_3D ( 'NONE', #9005, #14510, #16172 ) ;
#6078 = CARTESIAN_POINT ( 'NONE',  ( -22.42941481617252109, 36.22509709906984199, -139.9955747711319702 ) ) ;
#6079 = CARTESIAN_POINT ( 'NONE',  ( -30.57243748982824982, 40.56622750711377279, -145.3687906872534654 ) ) ;
#6080 = CIRCLE ( 'NONE', #22036, 8.000000000000000000 ) ;
#6081 = VECTOR ( 'NONE', #21532, 1000.000000000000000 ) ;
#6082 = CARTESIAN_POINT ( 'NONE',  ( -9.873006318519999880, -23.84776512999999909, -143.0552959529999839 ) ) ;
#6083 = DIRECTION ( 'NONE',  ( 2.507771768019999718E-12, 1.592654864069999939E-17, -1.000000000000000000 ) ) ;
#6084 = VERTEX_POINT ( 'NONE', #21040 ) ;
#6085 = DIRECTION ( 'NONE',  ( 1.000000000000000000, 0.000000000000000000, 0.000000000000000000 ) ) ;
#6086 = LINE ( 'NONE', #17019, #12348 ) ;
#6087 = CARTESIAN_POINT ( 'NONE',  ( -16.50000000000000711, -42.80091057724988701, -150.0552959530000123 ) ) ;
#6088 = CARTESIAN_POINT ( 'NONE',  ( 6.500000000130000011, 20.50000000000000000, -150.5552959529999839 ) ) ;
#6089 = FACE_OUTER_BOUND ( 'NONE', #309, .T. ) ;
#6090 = CARTESIAN_POINT ( 'NONE',  ( -15.05377294108086517, 35.21183796446418057, -147.7020849018581146 ) ) ;
#6091 = CARTESIAN_POINT ( 'NONE',  ( -17.18002735256251512, 36.98113687425442464, -140.6755148967337448 ) ) ;
#6092 = DIRECTION ( 'NONE',  ( 1.000000000000000000, 0.000000000000000000, -8.953948693601887499E-12 ) ) ;
#6093 = LINE ( 'NONE', #4196, #12986 ) ;
#6094 = FACE_OUTER_BOUND ( 'NONE', #7687, .T. ) ;
#6095 = AXIS2_PLACEMENT_3D ( 'NONE', #5229, #3457, #10804 ) ;
#6096 = AXIS2_PLACEMENT_3D ( 'NONE', #8715, #6948, #23484 ) ;
#6097 = ORIENTED_EDGE ( 'NONE', *, *, #3585, .T. ) ;
#6098 = CARTESIAN_POINT ( 'NONE',  ( -10.10076658436545216, 34.84004213900681890, -146.8689366150676960 ) ) ;
#6099 = FACE_BOUND ( 'NONE', #1758, .T. ) ;
#6100 = ORIENTED_EDGE ( 'NONE', *, *, #4204, .F. ) ;
#6101 = EDGE_CURVE ( 'NONE', #15239, #14839, #15578, .T. ) ;
#6102 = CARTESIAN_POINT ( 'NONE',  ( -22.37635798571903223, 34.72418241744752976, -147.2189273405841732 ) ) ;
#6103 = CARTESIAN_POINT ( 'NONE',  ( -3.499999999949999996, 31.50000000000000000, -150.0552959529999839 ) ) ;
#6104 = ORIENTED_EDGE ( 'NONE', *, *, #8207, .F. ) ;
#6105 = CARTESIAN_POINT ( 'NONE',  ( -12.82588262004118818, 32.50735092710331031, -143.6846524684992232 ) ) ;
#6106 = DIRECTION ( 'NONE',  ( -2.507771768019999718E-12, -1.592654864209999947E-17, 1.000000000000000000 ) ) ;
#6107 = CARTESIAN_POINT ( 'NONE',  ( 2.742326387956447231, 13.99062889862865156, -150.0552959529999839 ) ) ;
#6108 = CARTESIAN_POINT ( 'NONE',  ( -26.92552552937695154, 36.92880110468701105, -148.2769915172783328 ) ) ;
#6109 = CARTESIAN_POINT ( 'NONE',  ( 1.591914056710000080, -18.48847405160000079, -143.5552959529999839 ) ) ;
#6110 = MECHANICAL_DESIGN_GEOMETRIC_PRESENTATION_REPRESENTATION (  '', ( #21327 ), #9135 ) ;
#6111 = FACE_OUTER_BOUND ( 'NONE', #21017, .T. ) ;
#6112 = ORIENTED_EDGE ( 'NONE', *, *, #9665, .F. ) ;
#6113 = CARTESIAN_POINT ( 'NONE',  ( -28.16296462212046947, 36.26993904298343807, -147.8125575884918703 ) ) ;
#6114 = ORIENTED_EDGE ( 'NONE', *, *, #23106, .T. ) ;
#6115 = CARTESIAN_POINT ( 'NONE',  ( -14.40594365123728693, 36.16454659438798558, -140.4790970264384953 ) ) ;
#6116 = LINE ( 'NONE', #18846, #12202 ) ;
#6117 = DIRECTION ( 'NONE',  ( -0.9954742291034677226, 0.09503188512734457583, 4.503697062742119365E-12 ) ) ;
#6118 = ORIENTED_EDGE ( 'NONE', *, *, #9151, .T. ) ;
#6119 = DIRECTION ( 'NONE',  ( 1.000000000000000000, -1.190078432789999897E-50, -2.257144641399999941E-12 ) ) ;
#6120 = CARTESIAN_POINT ( 'NONE',  ( -9.347107914279998653, -17.32706600430000066, -144.5552959529999839 ) ) ;
#6121 = VECTOR ( 'NONE', #20773, 1000.000000000000227 ) ;
#6122 = CLOSED_SHELL ( 'NONE', ( #22066, #1078, #20319, #14625, #22671, #6006 ) ) ;
#6123 = VERTEX_POINT ( 'NONE', #933 ) ;
#6124 = AXIS2_PLACEMENT_3D ( 'NONE', #20055, #16371, #10753 ) ;
#6125 = CARTESIAN_POINT ( 'NONE',  ( -20.66689333112363869, 40.05648423817540760, -142.3232910573508150 ) ) ;
#6126 = EDGE_CURVE ( 'NONE', #18702, #14107, #6626, .T. ) ;
#6127 = CARTESIAN_POINT ( 'NONE',  ( 9.348856789759086183, 38.23672351627273969, -141.8825763927054311 ) ) ;
#6128 = EDGE_CURVE ( 'NONE', #22716, #990, #13889, .T. ) ;
#6129 = FACE_BOUND ( 'NONE', #21175, .T. ) ;
#6130 = CARTESIAN_POINT ( 'NONE',  ( 31.50000000000000000, 0.000000000000000000, -136.0552959530000123 ) ) ;
#6131 = CARTESIAN_POINT ( 'NONE',  ( -24.39187863320301730, 34.86260241805631921, -146.9285476356863285 ) ) ;
#6132 = ORIENTED_EDGE ( 'NONE', *, *, #12829, .T. ) ;
#6133 = CARTESIAN_POINT ( 'NONE',  ( 32.00000000000000000, -21.03620104879999886, -137.0552959530000123 ) ) ;
#6134 = VERTEX_POINT ( 'NONE', #14002 ) ;
#6135 = DIRECTION ( 'NONE',  ( 0.7071067811865499042, -0.7071067811865451302, 1.776356839400251071E-12 ) ) ;
#6136 = VECTOR ( 'NONE', #8553, 1000.000000000000000 ) ;
#6137 = VECTOR ( 'NONE', #11195, 1000.000000000000000 ) ;
#6138 = VECTOR ( 'NONE', #21959, 1000.000000000000000 ) ;
#6139 = EDGE_LOOP ( 'NONE', ( #18887, #8049, #21415, #14285 ) ) ;
#6140 =( LENGTH_UNIT ( ) NAMED_UNIT ( * ) SI_UNIT ( .MILLI., .METRE. ) );
#6141 = EDGE_LOOP ( 'NONE', ( #19135, #12048, #21068, #2905 ) ) ;
#6142 = LINE ( 'NONE', #6496, #8315 ) ;
#6143 = ORIENTED_EDGE ( 'NONE', *, *, #17903, .T. ) ;
#6144 = CARTESIAN_POINT ( 'NONE',  ( 25.31684607429999900, -45.26810052439999765, -136.0552959530000123 ) ) ;
#6145 = VERTEX_POINT ( 'NONE', #9827 ) ;
#6146 = EDGE_CURVE ( 'NONE', #968, #18797, #822, .T. ) ;
#6147 = ORIENTED_EDGE ( 'NONE', *, *, #5999, .T. ) ;
#6148 = CARTESIAN_POINT ( 'NONE',  ( -27.16475626468855964, 37.90277890276032480, -148.4897851378476048 ) ) ;
#6149 = LINE ( 'NONE', #5911, #10990 ) ;
#6150 = DIRECTION ( 'NONE',  ( -1.387778780781445676E-15, 1.000000000000000000, 0.000000000000000000 ) ) ;
#6151 = CARTESIAN_POINT ( 'NONE',  ( -32.50000000000000000, 26.00000000000000000, -146.5552959529999839 ) ) ;
#6152 = SHAPE_REPRESENTATION ( 'Latch Shaft Screw', ( #5025 ), #5779 ) ;
#6153 = CARTESIAN_POINT ( 'NONE',  ( -6.272593219194217085, 34.41819306988834626, -147.6053705869175019 ) ) ;
#6154 = CARTESIAN_POINT ( 'NONE',  ( -9.197324267851360702, 40.96642299144375698, -143.5436038170500126 ) ) ;
#6155 = ORIENTED_EDGE ( 'NONE', *, *, #4400, .T. ) ;
#6156 = LINE ( 'NONE', #7812, #20854 ) ;
#6157 = AXIS2_PLACEMENT_3D ( 'NONE', #5818, #22241, #2151 ) ;
#6158 = AXIS2_PLACEMENT_3D ( 'NONE', #19172, #12022, #11780 ) ;
#6159 = CARTESIAN_POINT ( 'NONE',  ( 9.293598222543803189, 38.27417067585172816, -146.2064413145477317 ) ) ;
#6160 = CARTESIAN_POINT ( 'NONE',  ( 3.742473698254299652, -2.190250522973148595, -136.0552959530084536 ) ) ;
#6161 = ORIENTED_EDGE ( 'NONE', *, *, #19673, .F. ) ;
#6162 = EDGE_CURVE ( 'NONE', #12155, #21927, #22582, .T. ) ;
#6163 = CARTESIAN_POINT ( 'NONE',  ( 16.26251912989999937, -22.62374141290000296, -143.5552959529999839 ) ) ;
#6164 = FACE_OUTER_BOUND ( 'NONE', #16658, .T. ) ;
#6165 = EDGE_LOOP ( 'NONE', ( #14502, #11106, #20432, #855 ) ) ;
#6166 = DIRECTION ( 'NONE',  ( -1.000000000000000000, 0.000000000000000000, 0.000000000000000000 ) ) ;
#6167 = CARTESIAN_POINT ( 'NONE',  ( -9.394779979509999990, -17.86685386420000299, -143.5552959529999839 ) ) ;
#6168 = ORIENTED_EDGE ( 'NONE', *, *, #18589, .T. ) ;
#6169 = LINE ( 'NONE', #11393, #19766 ) ;
#6170 = LINE ( 'NONE', #13421, #12610 ) ;
#6171 = ORIENTED_EDGE ( 'NONE', *, *, #8046, .F. ) ;
#6172 = FACE_OUTER_BOUND ( 'NONE', #17970, .T. ) ;
#6173 = CARTESIAN_POINT ( 'NONE',  ( -20.22605346220231937, 41.30495387708683097, -144.6507171862060090 ) ) ;
#6174 = COLOUR_RGB ( '', 0.72549020, 0.75294118, 0.79215686) ;
#6175 = ORIENTED_EDGE ( 'NONE', *, *, #23106, .F. ) ;
#6176 = SURFACE_SIDE_STYLE ('',( #21057 ) ) ;
#6177 = CIRCLE ( 'NONE', #17974, 35.00000000000000000 ) ;
#6178 = CARTESIAN_POINT ( 'NONE',  ( -28.37825339590731843, 32.94869610818383876, -141.6352474658662004 ) ) ;
#6179 = EDGE_CURVE ( 'NONE', #11337, #14361, #2828, .T. ) ;
#6180 = CARTESIAN_POINT ( 'NONE',  ( -2.499999999859999988, 31.00000000000000000, -146.5552959529999839 ) ) ;
#6181 = EDGE_LOOP ( 'NONE', ( #21491, #5511, #16663, #14229 ) ) ;
#6182 = DIRECTION ( 'NONE',  ( 0.000000000000000000, 1.000000000000000000, 0.000000000000000000 ) ) ;
#6183 = ADVANCED_FACE ( 'NONE', ( #17337 ), #1050, .F. ) ;
#6184 = DIRECTION ( 'NONE',  ( -1.000000000000000000, 0.000000000000000000, 2.257144641399999941E-12 ) ) ;
#6185 = VERTEX_POINT ( 'NONE', #12441 ) ;
#6186 = CARTESIAN_POINT ( 'NONE',  ( -10.07619956200000111, 36.21908991349999951, -147.8536995439999941 ) ) ;
#6187 = EDGE_CURVE ( 'NONE', #18415, #6658, #18167, .T. ) ;
#6188 = VERTEX_POINT ( 'NONE', #12213 ) ;
#6189 = DIRECTION ( 'NONE',  ( 1.526468026909999897E-13, 8.159623473500000156E-13, 1.000000000000000000 ) ) ;
#6190 = ADVANCED_FACE ( 'NONE', ( #5320 ), #12326, .F. ) ;
#6191 = DIRECTION ( 'NONE',  ( -1.000000000000000000, 0.000000000000000000, 2.257144641399999941E-12 ) ) ;
#6192 = VERTEX_POINT ( 'NONE', #1882 ) ;
#6193 = ORIENTED_EDGE ( 'NONE', *, *, #17787, .T. ) ;
#6194 = DIRECTION ( 'NONE',  ( 0.000000000000000000, 0.000000000000000000, 1.000000000000000000 ) ) ;
#6195 = CARTESIAN_POINT ( 'NONE',  ( -30.49999999990000177, 37.00000000000000000, -144.0552959529999839 ) ) ;
#6196 = DIRECTION ( 'NONE',  ( 0.000000000000000000, -1.000000000000000000, 0.000000000000000000 ) ) ;
#6197 = CARTESIAN_POINT ( 'NONE',  ( -8.296392858609999976, -9.821782169089999570, -148.5552959529999839 ) ) ;
#6198 = ORIENTED_EDGE ( 'NONE', *, *, #1029, .T. ) ;
#6199 = LINE ( 'NONE', #22266, #11656 ) ;
#6200 = PLANE ( 'NONE',  #17302 ) ;
#6201 = EDGE_CURVE ( 'NONE', #22505, #12665, #19718, .T. ) ;
#6202 = CARTESIAN_POINT ( 'NONE',  ( 12.77456842470000176, -18.14116071520000162, -143.5552959529999839 ) ) ;
#6203 = CARTESIAN_POINT ( 'NONE',  ( 13.66051412338692295, 38.90191174485966741, -136.0552959530308783 ) ) ;
#6204 = CARTESIAN_POINT ( 'NONE',  ( -25.10891061333510166, 37.07005729393355864, -148.1636427046707070 ) ) ;
#6205 = CARTESIAN_POINT ( 'NONE',  ( -15.55493608092991131, 33.62053755351711715, -145.7762437450627431 ) ) ;
#6206 = EDGE_CURVE ( 'NONE', #11246, #1657, #5193, .T. ) ;
#6207 = DIRECTION ( 'NONE',  ( 1.000000000000000000, 0.000000000000000000, 0.000000000000000000 ) ) ;
#6208 = EDGE_CURVE ( 'NONE', #14014, #8887, #12517, .T. ) ;
#6209 = CARTESIAN_POINT ( 'NONE',  ( -19.91220883949999987, 32.96944242089999477, -141.9853941000000077 ) ) ;
#6210 = CARTESIAN_POINT ( 'NONE',  ( -10.00000000000000000, 42.50000000000000000, -151.0552959529999839 ) ) ;
#6211 = PRODUCT_DEFINITION_FORMATION_WITH_SPECIFIED_SOURCE ( 'ANY', '', #4218, .NOT_KNOWN. ) ;
#6212 = CARTESIAN_POINT ( 'NONE',  ( -7.816799939239999162, -1.500000000000000000, -149.3052959529999839 ) ) ;
#6213 = ORIENTED_EDGE ( 'NONE', *, *, #19853, .F. ) ;
#6214 = CARTESIAN_POINT ( 'NONE',  ( -22.10824191589999899, -4.000000000000000000, -146.2257682199999920 ) ) ;
#6215 = DIRECTION ( 'NONE',  ( 0.000000000000000000, 0.000000000000000000, 1.000000000000000000 ) ) ;
#6216 = PLANE ( 'NONE',  #12465 ) ;
#6217 = EDGE_LOOP ( 'NONE', ( #21375, #4397, #21632, #13982, #224, #22296, #17476 ) ) ;
#6218 =( LENGTH_UNIT ( ) NAMED_UNIT ( * ) SI_UNIT ( .MILLI., .METRE. ) );
#6219 = CARTESIAN_POINT ( 'NONE',  ( -22.03156944975851772, 33.39557638515176308, -141.8445571065512070 ) ) ;
#6220 = CARTESIAN_POINT ( 'NONE',  ( 10.50000000010000001, 24.50000000000000000, -143.5552959529999839 ) ) ;
#6221 = ORIENTED_EDGE ( 'NONE', *, *, #10078, .T. ) ;
#6222 = CARTESIAN_POINT ( 'NONE',  ( -22.89493301684351678, 37.73932509630494536, -140.7085940212591595 ) ) ;
#6223 = CARTESIAN_POINT ( 'NONE',  ( -1.000000000000000222, 20.00701398444616785, -150.0552959529999839 ) ) ;
#6224 = DIRECTION ( 'NONE',  ( 0.000000000000000000, 0.000000000000000000, -1.000000000000000000 ) ) ;
#6225 = DIRECTION ( 'NONE',  ( 0.000000000000000000, -1.000000000000000000, 0.000000000000000000 ) ) ;
#6226 = FACE_OUTER_BOUND ( 'NONE', #16747, .T. ) ;
#6227 = CARTESIAN_POINT ( 'NONE',  ( -8.657020695883439032, 38.42035764118494967, -140.6896201932340773 ) ) ;
#6228 = VERTEX_POINT ( 'NONE', #23524 ) ;
#6229 = CARTESIAN_POINT ( 'NONE',  ( -28.07061429630000049, 34.82490105569999628, -147.0351741510000068 ) ) ;
#6230 =( NAMED_UNIT ( * ) PLANE_ANGLE_UNIT ( ) SI_UNIT ( $, .RADIAN. ) );
#6231 = ADVANCED_FACE ( 'NONE', ( #7101 ), #10769, .F. ) ;
#6232 = EDGE_CURVE ( 'NONE', #21515, #21976, #3540, .T. ) ;
#6233 = ORIENTED_EDGE ( 'NONE', *, *, #22414, .T. ) ;
#6234 = CARTESIAN_POINT ( 'NONE',  ( -13.37265858230000148, 32.83955069500000690, -141.7941727500000013 ) ) ;
#6235 = CARTESIAN_POINT ( 'NONE',  ( -6.683153925719999222, -50.50000000000000000, -150.0552959529999839 ) ) ;
#6236 = LINE ( 'NONE', #18848, #11141 ) ;
#6237 = EDGE_LOOP ( 'NONE', ( #17727, #6523, #19912, #20247 ) ) ;
#6238 = CARTESIAN_POINT ( 'NONE',  ( -3.499999999969999998, 44.50000000000000000, -137.0552959530000123 ) ) ;
#6239 = DIRECTION ( 'NONE',  ( 2.257305453670000045E-12, 0.000000000000000000, 1.000000000000000000 ) ) ;
#6240 = EDGE_LOOP ( 'NONE', ( #8866, #15575, #2931, #3867 ) ) ;
#6241 = DIRECTION ( 'NONE',  ( -1.000000000000000000, 0.000000000000000000, 0.000000000000000000 ) ) ;
#6242 = AXIS2_PLACEMENT_3D ( 'NONE', #23014, #22902, #6587 ) ;
#6243 = CARTESIAN_POINT ( 'NONE',  ( -18.37171575634234699, 40.97338532158482138, -143.4834898677627564 ) ) ;
#6244 = CARTESIAN_POINT ( 'NONE',  ( 7.810046034465172760, 35.66771806836383263, -146.1707627155566911 ) ) ;
#6245 = DIRECTION ( 'NONE',  ( -1.000000000000000000, 5.094701932209999624E-24, 0.000000000000000000 ) ) ;
#6246 = CARTESIAN_POINT ( 'NONE',  ( -25.64792992871111821, 37.04465132566619445, -139.7265440085400030 ) ) ;
#6247 = CARTESIAN_POINT ( 'NONE',  ( 3.038350857853684861, -3.890616787572018342, -150.0552959529999839 ) ) ;
#6248 = ORIENTED_EDGE ( 'NONE', *, *, #14188, .F. ) ;
#6249 = PLANE ( 'NONE',  #7285 ) ;
#6250 = EDGE_LOOP ( 'NONE', ( #1586, #15580, #1333, #8573, #17595, #8917, #5789, #22171 ) ) ;
#6251 = CARTESIAN_POINT ( 'NONE',  ( -9.347107914279998653, -17.32706600430000066, -144.5552959529999839 ) ) ;
#6252 = ORIENTED_EDGE ( 'NONE', *, *, #22, .T. ) ;
#6253 = DIRECTION ( 'NONE',  ( 0.000000000000000000, 1.000000000000000000, 0.000000000000000000 ) ) ;
#6254 = ORIENTED_EDGE ( 'NONE', *, *, #13885, .T. ) ;
#6255 = EDGE_CURVE ( 'NONE', #3916, #11473, #13277, .T. ) ;
#6256 = CARTESIAN_POINT ( 'NONE',  ( 6.500000000159999125, 20.50000000000000000, -140.5552959529999839 ) ) ;
#6257 = EDGE_LOOP ( 'NONE', ( #4225, #18147, #7179, #21923 ) ) ;
#6258 = CARTESIAN_POINT ( 'NONE',  ( 13.13369214859999978, -50.50000000000000000, -143.0552959529999839 ) ) ;
#6259 = EDGE_CURVE ( 'NONE', #11025, #14032, #3406, .T. ) ;
#6260 = ORIENTED_EDGE ( 'NONE', *, *, #14724, .T. ) ;
#6261 = ORIENTED_EDGE ( 'NONE', *, *, #20022, .T. ) ;
#6262 = DIRECTION ( 'NONE',  ( 0.9915498581664488054, 0.1297261684090585954, -4.315191440381949291E-12 ) ) ;
#6263 = DIRECTION ( 'NONE',  ( -0.07970438983373200059, -0.9968185442904001770, 8.265980492683321082E-13 ) ) ;
#6264 = CARTESIAN_POINT ( 'NONE',  ( -10.43323856990612875, 37.07027821888497954, -139.9576636760149313 ) ) ;
#6265 = CARTESIAN_POINT ( 'NONE',  ( -12.76385253890000016, 37.02886902030000016, -147.6186336929999925 ) ) ;
#6266 = CARTESIAN_POINT ( 'NONE',  ( -13.86630785140000022, 50.50000000000000000, -137.0552959530000123 ) ) ;
#6267 = CARTESIAN_POINT ( 'NONE',  ( -9.953901650897908127, 37.05155446197428404, -148.5872971972359551 ) ) ;
#6268 = VERTEX_POINT ( 'NONE', #14128 ) ;
#6269 = CARTESIAN_POINT ( 'NONE',  ( -6.683153925719999222, -50.50000000000000000, -136.0552959530000123 ) ) ;
#6270 = DIRECTION ( 'NONE',  ( -2.602084747549999882E-17, 1.000000000000000000, 5.873289694040000105E-29 ) ) ;
#6271 = CARTESIAN_POINT ( 'NONE',  ( 22.89765167458959283, 39.50000000000000000, -150.0552959530000123 ) ) ;
#6272 = ORIENTED_EDGE ( 'NONE', *, *, #10212, .T. ) ;
#6273 = AXIS2_PLACEMENT_3D ( 'NONE', #813, #17211, #13772 ) ;
#6274 = LINE ( 'NONE', #22350, #10148 ) ;
#6275 = CARTESIAN_POINT ( 'NONE',  ( 6.500000000149999124, 20.50000000000000000, -143.5552959529999839 ) ) ;
#6276 = ORIENTED_EDGE ( 'NONE', *, *, #18687, .F. ) ;
#6277 = LINE ( 'NONE', #831, #11305 ) ;
#6278 = DIRECTION ( 'NONE',  ( -0.9847555042252370550, 0.1739442350240419932, 0.000000000000000000 ) ) ;
#6279 = VERTEX_POINT ( 'NONE', #19602 ) ;
#6280 = DIRECTION ( 'NONE',  ( -0.9953753789357124848, 0.09606172499277225441, 7.355811845627876534E-14 ) ) ;
#6281 = CARTESIAN_POINT ( 'NONE',  ( 23.10730091830129140, -23.50000000000000355, -150.0552959529999839 ) ) ;
#6282 = ORIENTED_EDGE ( 'NONE', *, *, #18279, .T. ) ;
#6283 = LINE ( 'NONE', #15338, #1506 ) ;
#6284 = CARTESIAN_POINT ( 'NONE',  ( -24.42715506630251454, 35.06635613588049694, -148.3612119513088885 ) ) ;
#6285 = ADVANCED_FACE ( 'NONE', ( #7224 ), #9107, .F. ) ;
#6286 = ORIENTED_EDGE ( 'NONE', *, *, #710, .T. ) ;
#6287 =( BOUNDED_CURVE ( )  B_SPLINE_CURVE ( 5, ( #1818, #10822, #3597, #7928, #2485, #1704 ),
 .UNSPECIFIED., .F., .F. ) 
 B_SPLINE_CURVE_WITH_KNOTS ( ( 6, 6 ),
 ( 0.000000000000000000, 1.570796326807921472 ),
 .UNSPECIFIED. ) 
 CURVE ( )  GEOMETRIC_REPRESENTATION_ITEM ( )  RATIONAL_B_SPLINE_CURVE ( ( 1.000000000000000000, 0.5999999999967096098, 0.3999999999967095987, 0.2999999999975321852, 0.2499999999983548160, 0.2500000000000000000 ) ) 
 REPRESENTATION_ITEM ( '' )  );
#6288 = LINE ( 'NONE', #8068, #21304 ) ;
#6289 = ORIENTED_EDGE ( 'NONE', *, *, #15028, .F. ) ;
#6290 = FACE_BOUND ( 'NONE', #18411, .T. ) ;
#6291 = AXIS2_PLACEMENT_3D ( 'NONE', #15598, #17728, #3219 ) ;
#6292 = CARTESIAN_POINT ( 'NONE',  ( 24.11847952820000174, -31.58456057200000089, -143.5552959529999839 ) ) ;
#6293 = ORIENTED_EDGE ( 'NONE', *, *, #7650, .T. ) ;
#6294 = VECTOR ( 'NONE', #909, 1000.000000000000000 ) ;
#6295 = LINE ( 'NONE', #8185, #18616 ) ;
#6296 = ORIENTED_EDGE ( 'NONE', *, *, #1398, .F. ) ;
#6297 = CARTESIAN_POINT ( 'NONE',  ( 11.18859344972421788, -19.62717558213227420, -148.5552959529999555 ) ) ;
#6298 = EDGE_CURVE ( 'NONE', #7247, #21766, #16386, .T. ) ;
#6299 = CARTESIAN_POINT ( 'NONE',  ( -14.47770030809999930, -1.500000000000000000, -150.0552959529999839 ) ) ;
#6300 = ORIENTED_EDGE ( 'NONE', *, *, #15268, .T. ) ;
#6301 = VERTEX_POINT ( 'NONE', #21511 ) ;
#6302 = CARTESIAN_POINT ( 'NONE',  ( 23.89222110089999873, -31.59487100459999809, -146.5552959529999839 ) ) ;
#6303 = ADVANCED_FACE ( 'NONE', ( #10654 ), #14597, .T. ) ;
#6304 = LINE ( 'NONE', #13557, #8144 ) ;
#6305 = FACE_OUTER_BOUND ( 'NONE', #16005, .T. ) ;
#6306 = DIRECTION ( 'NONE',  ( 1.000000000000000000, 0.000000000000000000, -4.510774274160000731E-12 ) ) ;
#6307 = VECTOR ( 'NONE', #15092, 1000.000000000000000 ) ;
#6308 = ORIENTED_EDGE ( 'NONE', *, *, #8344, .T. ) ;
#6309 = CIRCLE ( 'NONE', #16569, 0.7500000000000006661 ) ;
#6310 = CARTESIAN_POINT ( 'NONE',  ( 19.16617820230000291, 49.81753540199999719, -149.5552959529999839 ) ) ;
#6311 = EDGE_CURVE ( 'NONE', #19314, #9544, #17695, .T. ) ;
#6312 = CARTESIAN_POINT ( 'NONE',  ( -16.30945103002074958, -42.24260211602405235, -150.0552959530000123 ) ) ;
#6313 = CARTESIAN_POINT ( 'NONE',  ( -31.50000000000000000, -43.00000000000000000, -149.5552959529999839 ) ) ;
#6314 = CARTESIAN_POINT ( 'NONE',  ( 31.50000000000000000, 39.80430157320000006, -150.0552959529999839 ) ) ;
#6315 = CARTESIAN_POINT ( 'NONE',  ( 0.3832000607639999834, -24.50000000000000000, -148.5552959529999839 ) ) ;
#6316 = CARTESIAN_POINT ( 'NONE',  ( -16.80500177779741122, 32.51593824403059330, -143.4123969145075534 ) ) ;
#6317 = CARTESIAN_POINT ( 'NONE',  ( -4.584402860569999127, 37.05223431090000474, -140.2914745300000163 ) ) ;
#6318 = DIRECTION ( 'NONE',  ( 1.000000000000000000, 0.000000000000000000, -8.955190032050000935E-12 ) ) ;
#6319 = CARTESIAN_POINT ( 'NONE',  ( -15.46250806109999942, -18.00000000000000000, -147.7289441310000200 ) ) ;
#6320 = ORIENTED_EDGE ( 'NONE', *, *, #8719, .T. ) ;
#6321 = CARTESIAN_POINT ( 'NONE',  ( -10.52090578602543758, 33.54316366365962665, -143.5130757456077504 ) ) ;
#6322 = DIRECTION ( 'NONE',  ( 2.255973186040000320E-12, 0.000000000000000000, 1.000000000000000000 ) ) ;
#6323 = EDGE_CURVE ( 'NONE', #16131, #13781, #8752, .T. ) ;
#6324 = AXIS2_PLACEMENT_3D ( 'NONE', #14799, #13006, #16118 ) ;
#6325 = DIRECTION ( 'NONE',  ( 1.526468026909860048E-13, 8.159623473498529972E-13, 1.000000000000000000 ) ) ;
#6326 = ORIENTED_EDGE ( 'NONE', *, *, #19836, .F. ) ;
#6327 = EDGE_CURVE ( 'NONE', #4645, #21739, #23291, .T. ) ;
#6328 = SURFACE_STYLE_USAGE ( .BOTH. , #17036 ) ;
#6329 = CARTESIAN_POINT ( 'NONE',  ( -22.19109655566130357, 33.58841674673155353, -143.6176153979714911 ) ) ;
#6330 = CARTESIAN_POINT ( 'NONE',  ( -15.00000000000000000, -44.50000000000000000, -136.5552959530000123 ) ) ;
#6331 = ORIENTED_EDGE ( 'NONE', *, *, #8469, .T. ) ;
#6332 = CARTESIAN_POINT ( 'NONE',  ( -23.82499398344462449, 40.43198470725418758, -143.7282993410326810 ) ) ;
#6333 = ADVANCED_FACE ( 'NONE', ( #8872 ), #18633, .T. ) ;
#6334 = DIRECTION ( 'NONE',  ( 1.000000000000000000, 0.000000000000000000, -2.253752739989067373E-12 ) ) ;
#6335 = ADVANCED_FACE ( 'NONE', ( #15055 ), #20069, .T. ) ;
#6336 = CARTESIAN_POINT ( 'NONE',  ( -0.2408409772196719867, 17.17512194927157410, -150.0552959529999839 ) ) ;
#6337 = LINE ( 'NONE', #10011, #3387 ) ;
#6338 = CARTESIAN_POINT ( 'NONE',  ( -10.14042191040790009, 37.07381867795185570, -148.2039739393879074 ) ) ;
#6339 = DIRECTION ( 'NONE',  ( 0.000000000000000000, -1.000000000000000000, -2.765629237170000203E-27 ) ) ;
#6340 = EDGE_CURVE ( 'NONE', #537, #2949, #21187, .T. ) ;
#6341 = CIRCLE ( 'NONE', #12803, 4.000000000000000000 ) ;
#6342 = CARTESIAN_POINT ( 'NONE',  ( 8.201139657833619978, -33.35711941572422745, -150.0552959529999839 ) ) ;
#6343 = ADVANCED_FACE ( 'NONE', ( #5890, #14705 ), #5778, .T. ) ;
#6344 = EDGE_LOOP ( 'NONE', ( #11566, #9276, #12901, #20824 ) ) ;
#6345 = CIRCLE ( 'NONE', #11640, 0.5000000000000004441 ) ;
#6346 = SURFACE_STYLE_FILL_AREA ( #15510 ) ;
#6347 = ORIENTED_EDGE ( 'NONE', *, *, #819, .T. ) ;
#6348 = CARTESIAN_POINT ( 'NONE',  ( -13.47165290112877933, 33.35876621949892495, -143.8174469061082164 ) ) ;
#6349 = DIRECTION ( 'NONE',  ( 0.000000000000000000, 0.000000000000000000, -1.000000000000000000 ) ) ;
#6350 = CARTESIAN_POINT ( 'NONE',  ( -4.565705854129999963, 38.02161370010000496, -148.1538225310000030 ) ) ;
#6351 = ORIENTED_EDGE ( 'NONE', *, *, #19721, .F. ) ;
#6352 = DIRECTION ( 'NONE',  ( 1.526468026909999897E-13, 8.159623473500000156E-13, 1.000000000000000000 ) ) ;
#6353 = CARTESIAN_POINT ( 'NONE',  ( -32.50000000000000000, 26.00000000000000000, -146.5552959529999839 ) ) ;
#6354 = ORIENTED_EDGE ( 'NONE', *, *, #5010, .F. ) ;
#6355 = CARTESIAN_POINT ( 'NONE',  ( -6.683153925719999222, -51.50000000000000000, -136.0552959530000123 ) ) ;
#6356 = AXIS2_PLACEMENT_3D ( 'NONE', #5255, #17752, #5134 ) ;
#6357 = CARTESIAN_POINT ( 'NONE',  ( -18.25771465379125758, 41.35085647821183841, -143.4491198483315202 ) ) ;
#6358 = VECTOR ( 'NONE', #7876, 1000.000000000000000 ) ;
#6359 = CARTESIAN_POINT ( 'NONE',  ( 7.587222251655057370, 35.80541937760241922, -146.2522771197009206 ) ) ;
#6360 = CYLINDRICAL_SURFACE ( 'NONE', #19978, 2.999999999999999112 ) ;
#6361 = EDGE_CURVE ( 'NONE', #21164, #4735, #1811, .T. ) ;
#6362 = CARTESIAN_POINT ( 'NONE',  ( -24.90252082163620173, 32.60880315492728698, -143.5690609613722017 ) ) ;
#6363 = DIRECTION ( 'NONE',  ( 5.094701932209999624E-24, 1.000000000000000000, 0.000000000000000000 ) ) ;
#6364 = ORIENTED_EDGE ( 'NONE', *, *, #18526, .F. ) ;
#6365 = CYLINDRICAL_SURFACE ( 'NONE', #13217, 0.7499999999999997780 ) ;
#6367 = ORIENTED_EDGE ( 'NONE', *, *, #21785, .T. ) ;
#6366 = VECTOR ( 'NONE', #11101, 1000.000000000000000 ) ;
#6368 = CARTESIAN_POINT ( 'NONE',  ( -26.92552552937697996, 36.92880110468703947, -148.2769915172784181 ) ) ;
#6369 = ORIENTED_EDGE ( 'NONE', *, *, #854, .T. ) ;
#6370 = PLANE ( 'NONE',  #731 ) ;
#6371 = VECTOR ( 'NONE', #5475, 1000.000000000000000 ) ;
#6372 = ORIENTED_EDGE ( 'NONE', *, *, #10361, .T. ) ;
#6373 = LINE ( 'NONE', #15311, #19781 ) ;
#6374 = ORIENTED_EDGE ( 'NONE', *, *, #12755, .F. ) ;
#6375 = ORIENTED_EDGE ( 'NONE', *, *, #22694, .F. ) ;
#6376 = CARTESIAN_POINT ( 'NONE',  ( -9.347107914279998653, -17.32706600430000066, -143.5552959529999839 ) ) ;
#6377 = CARTESIAN_POINT ( 'NONE',  ( -18.18930989791016017, 36.96028804430739712, -147.6841622079794263 ) ) ;
#6378 = DIRECTION ( 'NONE',  ( -2.602084704489999637E-17, 1.000000000000000000, 4.426606872070000353E-37 ) ) ;
#6379 = LINE ( 'NONE', #11602, #3749 ) ;
#6380 = CARTESIAN_POINT ( 'NONE',  ( -7.856058713508018876, 37.01980778200626077, -139.4032252962329324 ) ) ;
#6381 = CARTESIAN_POINT ( 'NONE',  ( -9.971101149592600521, 37.05360750091987398, -147.8421425030599892 ) ) ;
#6382 = ORIENTED_EDGE ( 'NONE', *, *, #7070, .F. ) ;
#6383 = DIRECTION ( 'NONE',  ( -1.000000000000000000, 0.000000000000000000, 2.257120985840000117E-12 ) ) ;
#6384 = VECTOR ( 'NONE', #372, 1000.000000000000000 ) ;
#6385 = EDGE_CURVE ( 'NONE', #23438, #21392, #6008, .T. ) ;
#6386 = CARTESIAN_POINT ( 'NONE',  ( 9.689786586155861414, 36.08099448470404980, -146.3817958922141429 ) ) ;
#6387 = VECTOR ( 'NONE', #21637, 1000.000000000000000 ) ;
#6388 = DIRECTION ( 'NONE',  ( -1.000000000000000000, 0.000000000000000000, 0.000000000000000000 ) ) ;
#6389 = ADVANCED_FACE ( 'NONE', ( #3892 ), #20538, .F. ) ;
#6390 = ORIENTED_EDGE ( 'NONE', *, *, #11820, .T. ) ;
#6391 = CARTESIAN_POINT ( 'NONE',  ( -18.08788331829543949, 37.73304001162023980, -147.6923967947225833 ) ) ;
#6392 = DIRECTION ( 'NONE',  ( 1.000000000000000000, 0.000000000000000000, 2.507771768019999718E-12 ) ) ;
#6393 = VERTEX_POINT ( 'NONE', #9682 ) ;
#6394 = PLANE ( 'NONE',  #2134 ) ;
#6395 = ORIENTED_EDGE ( 'NONE', *, *, #21298, .T. ) ;
#6396 = CARTESIAN_POINT ( 'NONE',  ( -21.89685178209297334, 37.04474463554617358, -147.4979728338151119 ) ) ;
#6397 = CARTESIAN_POINT ( 'NONE',  ( -18.64767072899999789, 38.89869937459999960, -148.1651290810000319 ) ) ;
#6398 = EDGE_LOOP ( 'NONE', ( #9857, #14908, #1018, #14258 ) ) ;
#6399 = CARTESIAN_POINT ( 'NONE',  ( -14.60833405737009905, 37.68941485723577500, -140.4549841786794957 ) ) ;
#6400 = CARTESIAN_POINT ( 'NONE',  ( -25.12153080207939837, 33.08100675596072193, -141.7696838824860208 ) ) ;
#6401 = VERTEX_POINT ( 'NONE', #16958 ) ;
#6402 = AXIS2_PLACEMENT_3D ( 'NONE', #21156, #17216, #931 ) ;
#6403 = DIRECTION ( 'NONE',  ( 0.000000000000000000, 1.000000000000000000, 0.000000000000000000 ) ) ;
#6404 = VERTEX_POINT ( 'NONE', #20197 ) ;
#6405 = CARTESIAN_POINT ( 'NONE',  ( 6.500000000140000012, 20.50000000000000000, -147.0552959529999839 ) ) ;
#6406 = AXIS2_PLACEMENT_3D ( 'NONE', #1928, #1447, #5589 ) ;
#6407 = DIRECTION ( 'NONE',  ( -2.507771768022264771E-12, -1.592655090489709912E-17, 1.000000000000000000 ) ) ;
#6408 = ORIENTED_EDGE ( 'NONE', *, *, #21475, .T. ) ;
#6409 = DIRECTION ( 'NONE',  ( 2.257171095940000041E-12, 1.003664318210000046E-28, 1.000000000000000000 ) ) ;
#6410 = VECTOR ( 'NONE', #21522, 1000.000000000000000 ) ;
#6411 = EDGE_LOOP ( 'NONE', ( #6881, #708, #14928, #860 ) ) ;
#6412 = AXIS2_PLACEMENT_3D ( 'NONE', #21535, #19865, #3796 ) ;
#6413 = CARTESIAN_POINT ( 'NONE',  ( 6.000000000160000013, 36.50000000000000000, -140.5552959529999839 ) ) ;
#6414 = LINE ( 'NONE', #1207, #20872 ) ;
#6415 = ORIENTED_EDGE ( 'NONE', *, *, #9056, .F. ) ;
#6416 = EDGE_CURVE ( 'NONE', #9000, #4474, #11146, .T. ) ;
#6417 = EDGE_CURVE ( 'NONE', #17085, #7870, #7787, .T. ) ;
#6418 = ORIENTED_EDGE ( 'NONE', *, *, #16781, .F. ) ;
#6419 = CARTESIAN_POINT ( 'NONE',  ( 6.500000000140000012, 20.50000000000000000, -147.5552959529999839 ) ) ;
#6420 = VECTOR ( 'NONE', #21335, 1000.000000000000000 ) ;
#6421 = CARTESIAN_POINT ( 'NONE',  ( 5.347956485829999274, -22.34165470570000167, -147.5552959529999839 ) ) ;
#6422 = AXIS2_PLACEMENT_3D ( 'NONE', #15804, #1195, #13901 ) ;
#6423 = CARTESIAN_POINT ( 'NONE',  ( -11.14725012360000100, -1.500000000000000000, -150.0552959529999839 ) ) ;
#6424 = DIRECTION ( 'NONE',  ( 4.510774274160000731E-12, -1.321907670990000086E-13, 1.000000000000000000 ) ) ;
#6425 = ORIENTED_EDGE ( 'NONE', *, *, #19681, .F. ) ;
#6426 = DIRECTION ( 'NONE',  ( 1.211690350419999855E-27, 2.765629237170000203E-27, -1.000000000000000000 ) ) ;
#6427 = DIRECTION ( 'NONE',  ( 1.000000000000000000, 0.000000000000000000, 2.504899991129999675E-12 ) ) ;
#6428 =( BOUNDED_CURVE ( )  B_SPLINE_CURVE ( 5, ( #1701, #3471, #8920, #14760, #22027, #17869 ),
 .UNSPECIFIED., .F., .F. ) 
 B_SPLINE_CURVE_WITH_KNOTS ( ( 6, 6 ),
 ( 1.570796326769926310, 3.141592653590000062 ),
 .UNSPECIFIED. ) 
 CURVE ( )  GEOMETRIC_REPRESENTATION_ITEM ( )  RATIONAL_B_SPLINE_CURVE ( ( 0.2499999999999999445, 0.2499999999968074982, 0.2999999999952112639, 0.3999999999936150186, 0.5999999999936149742, 1.000000000000000000 ) ) 
 REPRESENTATION_ITEM ( '' )  );
#6429 = VECTOR ( 'NONE', #19170, 999.9999999999998863 ) ;
#6430 = CARTESIAN_POINT ( 'NONE',  ( 25.01085694111269930, -17.87864083493722944, -150.0552959529999839 ) ) ;
#6431 = CARTESIAN_POINT ( 'NONE',  ( -13.50000000000000000, -43.00000000000000000, -150.0552959529999839 ) ) ;
#6432 = CARTESIAN_POINT ( 'NONE',  ( -11.26413364422059082, 36.97109742518000530, -139.4278719022547079 ) ) ;
#6433 = AXIS2_PLACEMENT_3D ( 'NONE', #4028, #11151, #18424 ) ;
#6434 = CARTESIAN_POINT ( 'NONE',  ( -21.35824191589999899, -3.250000000000000000, -145.5657682190000060 ) ) ;
#6435 = ORIENTED_EDGE ( 'NONE', *, *, #22602, .F. ) ;
#6436 = FACE_OUTER_BOUND ( 'NONE', #14109, .T. ) ;
#6437 = CARTESIAN_POINT ( 'NONE',  ( 6.000000000140000012, 29.48610037779999971, -146.5552959529999839 ) ) ;
#6438 = CARTESIAN_POINT ( 'NONE',  ( -32.50000000000000000, 47.50000000000000000, -136.5552959530000123 ) ) ;
#6439 = FACE_OUTER_BOUND ( 'NONE', #7445, .T. ) ;
#6440 = CARTESIAN_POINT ( 'NONE',  ( -31.00000000000000000, 1.000000000000000000, -151.0552959529999839 ) ) ;
#6441 = AXIS2_PLACEMENT_3D ( 'NONE', #4969, #19492, #3186 ) ;
#6442 = EDGE_CURVE ( 'NONE', #20932, #12161, #9445, .T. ) ;
#6443 = ORIENTED_EDGE ( 'NONE', *, *, #8853, .F. ) ;
#6444 = CARTESIAN_POINT ( 'NONE',  ( -9.857095426776597336, 33.85551485821954287, -145.6647977573206560 ) ) ;
#6445 = FACE_OUTER_BOUND ( 'NONE', #939, .T. ) ;
#6446 = VECTOR ( 'NONE', #13559, 1000.000000000000000 ) ;
#6447 = CARTESIAN_POINT ( 'NONE',  ( 4.890549297259640937, -2.038177252827572339, -150.0552959529999839 ) ) ;
#6448 = EDGE_LOOP ( 'NONE', ( #5942, #1858, #13046, #337 ) ) ;
#6449 = LINE ( 'NONE', #19300, #13326 ) ;
#6450 = VECTOR ( 'NONE', #12340, 1000.000000000000000 ) ;
#6451 = VECTOR ( 'NONE', #16424, 1000.000000000000000 ) ;
#6452 = VECTOR ( 'NONE', #21559, 1000.000000000000000 ) ;
#6453 = CARTESIAN_POINT ( 'NONE',  ( -32.50000000000000000, 19.50000000000000000, -149.5552959529999839 ) ) ;
#6454 = ADVANCED_FACE ( 'NONE', ( #11123 ), #313, .F. ) ;
#6455 = DIRECTION ( 'NONE',  ( 0.000000000000000000, 0.000000000000000000, 1.000000000000000000 ) ) ;
#6456 = EDGE_LOOP ( 'NONE', ( #1004, #10179, #14601, #18644 ) ) ;
#6457 = CARTESIAN_POINT ( 'NONE',  ( -23.49236497903126164, 40.48720019302773210, -144.5163663921258603 ) ) ;
#6458 = DIRECTION ( 'NONE',  ( 1.000000000000000000, 0.000000000000000000, -2.253752739989067373E-12 ) ) ;
#6459 = CARTESIAN_POINT ( 'NONE',  ( 5.519360106948777656, 13.04803137664723423, -150.0552959530000123 ) ) ;
#6460 = CARTESIAN_POINT ( 'NONE',  ( 1.561837858109999866, -18.84848306830000197, -143.5552959529999839 ) ) ;
#6461 = CARTESIAN_POINT ( 'NONE',  ( -9.178237216079999428, 36.01795878010000251, -148.2568923610000127 ) ) ;
#6462 = LINE ( 'NONE', #13475, #21120 ) ;
#6463 = CARTESIAN_POINT ( 'NONE',  ( -7.977873771066918529, 39.10042569864757667, -141.2099287470478828 ) ) ;
#6464 = EDGE_CURVE ( 'NONE', #22304, #1069, #5550, .T. ) ;
#6465 = EDGE_LOOP ( 'NONE', ( #22973, #12741, #19625, #6100 ) ) ;
#6466 = VECTOR ( 'NONE', #6239, 1000.000000000000000 ) ;
#6467 = AXIS2_PLACEMENT_3D ( 'NONE', #13254, #655, #4101 ) ;
#6468 = DIRECTION ( 'NONE',  ( 2.257157423930000049E-12, 0.000000000000000000, 1.000000000000000000 ) ) ;
#6469 = CIRCLE ( 'NONE', #21999, 1.000000000000000888 ) ;
#6470 = VERTEX_POINT ( 'NONE', #9224 ) ;
#6471 = CARTESIAN_POINT ( 'NONE',  ( -6.998540199153231001, 33.60912705789826305, -142.1258228245172290 ) ) ;
#6472 = CARTESIAN_POINT ( 'NONE',  ( 19.77963439019999825, 51.26338628519999929, -136.0552959530000123 ) ) ;
#6473 = LINE ( 'NONE', #12398, #9638 ) ;
#6474 = EDGE_CURVE ( 'NONE', #17870, #8517, #16492, .T. ) ;
#6475 = VERTEX_POINT ( 'NONE', #13146 ) ;
#6476 = CARTESIAN_POINT ( 'NONE',  ( -35.07300000000000040, 11.44852983560000048, -143.5552959529999839 ) ) ;
#6477 = CARTESIAN_POINT ( 'NONE',  ( -32.50000000000000000, 46.00000000000000000, -144.0552959529999839 ) ) ;
#6478 = ADVANCED_FACE ( 'NONE', ( #2224 ), #14640, .F. ) ;
#6479 = ORIENTED_EDGE ( 'NONE', *, *, #3308, .T. ) ;
#6480 = CARTESIAN_POINT ( 'NONE',  ( -21.79874322595727421, 37.75473737279066455, -147.4889873734535399 ) ) ;
#6481 = EDGE_CURVE ( 'NONE', #10191, #19149, #8850, .T. ) ;
#6482 = EDGE_CURVE ( 'NONE', #11395, #11936, #8496, .T. ) ;
#6483 = CARTESIAN_POINT ( 'NONE',  ( -18.99860119798404412, 37.95224228446289061, -148.1887462952859096 ) ) ;
#6484 = CARTESIAN_POINT ( 'NONE',  ( -12.00000000000000000, -43.00000000000000000, -150.0552959529999839 ) ) ;
#6485 = VECTOR ( 'NONE', #18096, 1000.000000000000000 ) ;
#6486 = CARTESIAN_POINT ( 'NONE',  ( 7.039431774584924639, 36.65394157649679840, -146.5317159311551336 ) ) ;
#6487 = AXIS2_PLACEMENT_3D ( 'NONE', #16145, #1523, #8747 ) ;
#6488 = LINE ( 'NONE', #6130, #16926 ) ;
#6489 = CARTESIAN_POINT ( 'NONE',  ( -25.13189125417029501, 34.91836258124934744, -146.9977978136419949 ) ) ;
#6490 = CARTESIAN_POINT ( 'NONE',  ( 5.700859806000233121, -4.419886383052269885, -150.0552959530000123 ) ) ;
#6491 = CARTESIAN_POINT ( 'NONE',  ( -13.18072986969131932, 37.07863008620352474, -148.2345011165226651 ) ) ;
#6492 = ORIENTED_EDGE ( 'NONE', *, *, #13323, .T. ) ;
#6493 = DIRECTION ( 'NONE',  ( -0.9874789572432817186, 0.1577507813030449846, 0.000000000000000000 ) ) ;
#6494 = ORIENTED_EDGE ( 'NONE', *, *, #1742, .F. ) ;
#6495 = ORIENTED_EDGE ( 'NONE', *, *, #15071, .F. ) ;
#6496 = CARTESIAN_POINT ( 'NONE',  ( 31.50000000010000178, -40.03620104880000241, -136.5552959530000123 ) ) ;
#6497 = ORIENTED_EDGE ( 'NONE', *, *, #17383, .T. ) ;
#6498 = LINE ( 'NONE', #9810, #22816 ) ;
#6499 = VECTOR ( 'NONE', #6855, 1000.000000000000000 ) ;
#6500 = ORIENTED_EDGE ( 'NONE', *, *, #3308, .F. ) ;
#6501 = AXIS2_PLACEMENT_3D ( 'NONE', #16388, #14489, #12688 ) ;
#6502 = ADVANCED_FACE ( 'NONE', ( #19815 ), #12304, .F. ) ;
#6503 = ORIENTED_EDGE ( 'NONE', *, *, #21298, .F. ) ;
#6504 = DIRECTION ( 'NONE',  ( 0.000000000000000000, -1.000000000000000000, 0.000000000000000000 ) ) ;
#6505 = CARTESIAN_POINT ( 'NONE',  ( -18.66943014212572649, 35.65202800753842638, -147.2469133860827526 ) ) ;
#6506 = EDGE_CURVE ( 'NONE', #22598, #12804, #10743, .T. ) ;
#6507 = CARTESIAN_POINT ( 'NONE',  ( -10.65913935279999869, 37.04331329920000115, -139.7140392919999954 ) ) ;
#6508 = CARTESIAN_POINT ( 'NONE',  ( -6.812760379890000273, 32.88798608609999974, -143.6676051400000063 ) ) ;
#6509 = DIRECTION ( 'NONE',  ( 1.000000000000000000, 0.000000000000000000, -2.257560236040000027E-12 ) ) ;
#6510 = EDGE_LOOP ( 'NONE', ( #2733, #12339, #16089, #16614 ) ) ;
#6511 = CARTESIAN_POINT ( 'NONE',  ( -6.683153925719999222, 50.50000000000000000, -150.0552959529999839 ) ) ;
#6512 = CARTESIAN_POINT ( 'NONE',  ( 9.489186301925801814, 35.86813483702695038, -146.2857056571775729 ) ) ;
#6513 = CARTESIAN_POINT ( 'NONE',  ( -46.29070078840000235, 26.50000000000000000, -147.5552959529999839 ) ) ;
#6514 = CIRCLE ( 'NONE', #3114, 2.000000000000001776 ) ;
#6515 = ORIENTED_EDGE ( 'NONE', *, *, #78, .F. ) ;
#6516 = DIRECTION ( 'NONE',  ( 1.000000000000000000, 0.000000000000000000, -1.498801083243961330E-13 ) ) ;
#6517 = FACE_OUTER_BOUND ( 'NONE', #3350, .T. ) ;
#6518 = ORIENTED_EDGE ( 'NONE', *, *, #11582, .T. ) ;
#6519 = FACE_BOUND ( 'NONE', #6641, .T. ) ;
#6520 = ORIENTED_EDGE ( 'NONE', *, *, #3720, .T. ) ;
#6521 = FACE_OUTER_BOUND ( 'NONE', #14271, .T. ) ;
#6522 = CARTESIAN_POINT ( 'NONE',  ( 15.97954986339999905, -26.72957102550000030, -143.0552959529999839 ) ) ;
#6523 = ORIENTED_EDGE ( 'NONE', *, *, #13448, .T. ) ;
#6524 = CARTESIAN_POINT ( 'NONE',  ( -14.11967125435642068, 36.98834135279123814, -140.5455248811313993 ) ) ;
#6525 = CARTESIAN_POINT ( 'NONE',  ( -25.75289790537111045, 32.48043154014510492, -144.6283460670170768 ) ) ;
#6526 = VERTEX_POINT ( 'NONE', #1736 ) ;
#6527 = DIRECTION ( 'NONE',  ( -1.000000000000000000, 0.000000000000000000, 0.000000000000000000 ) ) ;
#6528 = ADVANCED_FACE ( 'NONE', ( #8722 ), #21601, .F. ) ;
#6529 = EDGE_LOOP ( 'NONE', ( #17919, #7385, #12798, #21642 ) ) ;
#6530 = DIRECTION ( 'NONE',  ( -0.09606172499277226828, -0.9953753789357124848, 8.268133652477615271E-13 ) ) ;
#6531 = DIRECTION ( 'NONE',  ( 1.527666881879999979E-13, 8.100187187669999987E-13, 1.000000000000000000 ) ) ;
#6532 = ORIENTED_EDGE ( 'NONE', *, *, #3582, .F. ) ;
#6533 = CARTESIAN_POINT ( 'NONE',  ( 32.50000000000000000, 39.92025131090000656, -150.0552959529999839 ) ) ;
#6534 = VECTOR ( 'NONE', #16564, 1000.000000000000000 ) ;
#6535 = AXIS2_PLACEMENT_3D ( 'NONE', #20495, #7632, #6092 ) ;
#6536 = VERTEX_POINT ( 'NONE', #17668 ) ;
#6537 = CARTESIAN_POINT ( 'NONE',  ( 23.84377886109999878, -30.60602870049999780, -145.0552959529999839 ) ) ;
#6538 = FACE_OUTER_BOUND ( 'NONE', #17624, .T. ) ;
#6539 = ORIENTED_EDGE ( 'NONE', *, *, #25, .F. ) ;
#6540 = ORIENTED_EDGE ( 'NONE', *, *, #3889, .F. ) ;
#6541 = LINE ( 'NONE', #15591, #12011 ) ;
#6542 = LINE ( 'NONE', #6421, #5884 ) ;
#6543 = CARTESIAN_POINT ( 'NONE',  ( -14.74965217832113851, 40.59671102096423567, -143.6490422507460210 ) ) ;
#6544 = CARTESIAN_POINT ( 'NONE',  ( -7.337311498550000088, -24.10744501490000147, -148.0552959529999839 ) ) ;
#6545 = VERTEX_POINT ( 'NONE', #16001 ) ;
#6546 = LINE ( 'NONE', #13814, #14364 ) ;
#6547 = DIRECTION ( 'NONE',  ( -1.000000000000000000, 0.000000000000000000, -2.508689552389999873E-12 ) ) ;
#6548 = VECTOR ( 'NONE', #6531, 1000.000000000000000 ) ;
#6549 = CARTESIAN_POINT ( 'NONE',  ( 21.65635984007525394, -18.10099947280546573, -150.0552959529999839 ) ) ;
#6550 = PLANE ( 'NONE',  #694 ) ;
#6551 = CARTESIAN_POINT ( 'NONE',  ( -32.50000000000000000, 15.91770215440000236, -140.5449657050000098 ) ) ;
#6552 = DIRECTION ( 'NONE',  ( 2.257144641399999941E-12, -8.049635416090000264E-35, 1.000000000000000000 ) ) ;
#6553 = ORIENTED_EDGE ( 'NONE', *, *, #9782, .T. ) ;
#6554 = LINE ( 'NONE', #13930, #17922 ) ;
#6555 = EDGE_CURVE ( 'NONE', #8640, #1, #14332, .T. ) ;
#6556 = DIRECTION ( 'NONE',  ( 4.510774274160000731E-12, -1.321907670990000086E-13, 1.000000000000000000 ) ) ;
#6557 = DIRECTION ( 'NONE',  ( 4.510774274160000731E-12, -1.321907670990000086E-13, 1.000000000000000000 ) ) ;
#6558 = CARTESIAN_POINT ( 'NONE',  ( -5.459597139290000456, 36.94776568910000236, -139.8191173760000083 ) ) ;
#6559 = ADVANCED_FACE ( 'NONE', ( #5284 ), #7188, .T. ) ;
#6560 = CARTESIAN_POINT ( 'NONE',  ( -30.99999999989999822, 37.00000000000000000, -138.5552959529999839 ) ) ;
#6561 = VERTEX_POINT ( 'NONE', #23262 ) ;
#6562 = CARTESIAN_POINT ( 'NONE',  ( -9.285539185979999388, 35.09287230280000358, -147.9937876190000168 ) ) ;
#6563 = DIRECTION ( 'NONE',  ( 2.839308199620000013E-14, 3.568879590630000244E-13, 1.000000000000000000 ) ) ;
#6564 = LINE ( 'NONE', #12265, #7534 ) ;
#6565 =( GEOMETRIC_REPRESENTATION_CONTEXT ( 3 ) GLOBAL_UNCERTAINTY_ASSIGNED_CONTEXT ( ( #2092 ) ) GLOBAL_UNIT_ASSIGNED_CONTEXT ( ( #8479, #23124, #7050 ) ) REPRESENTATION_CONTEXT ( 'NONE', 'WORKASPACE' ) );
#6566 = ORIENTED_EDGE ( 'NONE', *, *, #22379, .F. ) ;
#6567 = AXIS2_PLACEMENT_3D ( 'NONE', #4668, #2884, #21092 ) ;
#6568 = CARTESIAN_POINT ( 'NONE',  ( -10.00000000000000000, 19.50000000000000000, -151.0552959529999839 ) ) ;
#6569 = LINE ( 'NONE', #19067, #15555 ) ;
#6570 = LINE ( 'NONE', #10472, #14417 ) ;
#6571 = ORIENTED_EDGE ( 'NONE', *, *, #7497, .F. ) ;
#6572 = CARTESIAN_POINT ( 'NONE',  ( -22.48976697756137710, 37.06353063726883335, -140.4055699430226412 ) ) ;
#6573 = DIRECTION ( 'NONE',  ( 1.000000000000000000, 0.000000000000000000, 0.000000000000000000 ) ) ;
#6574 = CARTESIAN_POINT ( 'NONE',  ( 20.50000000000000000, 25.50000000000000000, -137.0552959530000123 ) ) ;
#6575 = CARTESIAN_POINT ( 'NONE',  ( 8.326040366162002826, 38.49009014742802037, -142.0478861723179023 ) ) ;
#6576 = CARTESIAN_POINT ( 'NONE',  ( -9.562013113524754360, 37.00477621356877478, -148.7272342976183381 ) ) ;
#6577 = DIRECTION ( 'NONE',  ( 0.000000000000000000, -1.000000000000000000, 0.000000000000000000 ) ) ;
#6578 = CARTESIAN_POINT ( 'NONE',  ( 4.204281436780199499, -34.38417682219860438, -150.0552959529999839 ) ) ;
#6579 = ORIENTED_EDGE ( 'NONE', *, *, #19941, .F. ) ;
#6580 = B_SPLINE_CURVE_WITH_KNOTS ( 'NONE', 5,
 ( #20378, #18716, #11307, #20618, #18584, #9403, #14905, #6209, #5737, #4313, #16914, #11542 ),
 .UNSPECIFIED., .F., .F.,
 ( 6, 3, 3, 6 ),
 ( 0.000000000000000000, 4.059123295939999210, 8.340116530639999581, 12.86134770560000007 ),
 .UNSPECIFIED. ) ;
#6581 = AXIS2_PLACEMENT_3D ( 'NONE', #23385, #22923, #10870 ) ;
#6582 = CARTESIAN_POINT ( 'NONE',  ( -21.03694116386247970, 36.94210036639699979, -147.9486865819903869 ) ) ;
#6583 = ORIENTED_EDGE ( 'NONE', *, *, #17066, .T. ) ;
#6584 = CARTESIAN_POINT ( 'NONE',  ( -8.262608331957180141, 35.43026936969504703, -140.7385567855430963 ) ) ;
#6585 = CARTESIAN_POINT ( 'NONE',  ( -29.55850978550000363, 41.47329217819999769, -142.4456950389999861 ) ) ;
#6586 = EDGE_CURVE ( 'NONE', #23020, #6018, #21724, .T. ) ;
#6587 = DIRECTION ( 'NONE',  ( 0.7071067811865473507, 0.7071067811865476838, -1.591319668629389897E-12 ) ) ;
#6588 = VERTEX_POINT ( 'NONE', #21484 ) ;
#6589 = DIRECTION ( 'NONE',  ( 1.000000000000000000, 0.000000000000000000, -4.429789868254373788E-12 ) ) ;
#6590 = DIRECTION ( 'NONE',  ( 1.000000000000000000, 0.000000000000000000, -1.701177084980000217E-20 ) ) ;
#6591 = ORIENTED_EDGE ( 'NONE', *, *, #23033, .T. ) ;
#6592 = CARTESIAN_POINT ( 'NONE',  ( -21.88274988998765735, 38.62264069534737843, -147.6131461927444377 ) ) ;
#6593 = EDGE_CURVE ( 'NONE', #4852, #2114, #7856, .T. ) ;
#6594 = CARTESIAN_POINT ( 'NONE',  ( -17.22605506639999717, 36.97564272059999979, -139.5994799229999899 ) ) ;
#6595 = LINE ( 'NONE', #10390, #21157 ) ;
#6596 = CARTESIAN_POINT ( 'NONE',  ( -32.50000000000000000, 48.00000000000000000, -150.5552959529999839 ) ) ;
#6597 = DIRECTION ( 'NONE',  ( 1.000000000000000000, 0.000000000000000000, -2.257453483404485639E-12 ) ) ;
#6598 = CARTESIAN_POINT ( 'NONE',  ( -24.79371418848295860, 32.62011804878908094, -144.5039952333927999 ) ) ;
#6599 = CARTESIAN_POINT ( 'NONE',  ( -33.50000000000000000, -74.00000000000000000, -155.5552959529999839 ) ) ;
#6600 = CYLINDRICAL_SURFACE ( 'NONE', #1783, 2.999999999999999112 ) ;
#6601 = EDGE_CURVE ( 'NONE', #20510, #19149, #9595, .T. ) ;
#6602 = ORIENTED_EDGE ( 'NONE', *, *, #12420, .T. ) ;
#6603 = DIRECTION ( 'NONE',  ( 2.257242012349999735E-12, 0.000000000000000000, -1.000000000000000000 ) ) ;
#6604 = UNCERTAINTY_MEASURE_WITH_UNIT (LENGTH_MEASURE( 1.000000000000000082E-05 ), #13530, 'distance_accuracy_value', 'NONE');
#6605 = EDGE_CURVE ( 'NONE', #21627, #4564, #15875, .T. ) ;
#6606 = ORIENTED_EDGE ( 'NONE', *, *, #18951, .F. ) ;
#6607 = ORIENTED_EDGE ( 'NONE', *, *, #1995, .T. ) ;
#6608 = ADVANCED_FACE ( 'NONE', ( #19686 ), #3383, .T. ) ;
#6609 = VERTEX_POINT ( 'NONE', #18263 ) ;
#6610 = DIRECTION ( 'NONE',  ( 0.9896415801065049367, -0.1435602414469282218, -8.993136838065500309E-12 ) ) ;
#6611 = CARTESIAN_POINT ( 'NONE',  ( -29.13601448249999848, 36.98639052360000079, -140.5419328609999923 ) ) ;
#6612 = ORIENTED_EDGE ( 'NONE', *, *, #11852, .T. ) ;
#6613 = ORIENTED_EDGE ( 'NONE', *, *, #21402, .T. ) ;
#6614 = VECTOR ( 'NONE', #21712, 1000.000000000000000 ) ;
#6615 = DIRECTION ( 'NONE',  ( 1.000000000000000000, 0.000000000000000000, 0.000000000000000000 ) ) ;
#6616 = CARTESIAN_POINT ( 'NONE',  ( -18.99756833806441492, 36.36014154320098157, -147.4937258815151608 ) ) ;
#6617 = DIRECTION ( 'NONE',  ( -1.211690350419999855E-27, -2.765629237170000203E-27, 1.000000000000000000 ) ) ;
#6618 = FACE_OUTER_BOUND ( 'NONE', #4810, .T. ) ;
#6619 = CARTESIAN_POINT ( 'NONE',  ( -7.344042119375912669, 32.21321104593293683, -144.7067442997065996 ) ) ;
#6620 = CARTESIAN_POINT ( 'NONE',  ( -9.007281809890079316, 38.87169400220813742, -148.3307225037476371 ) ) ;
#6621 = ORIENTED_EDGE ( 'NONE', *, *, #14621, .T. ) ;
#6622 = EDGE_CURVE ( 'NONE', #23525, #20598, #6341, .T. ) ;
#6623 = LINE ( 'NONE', #3072, #18206 ) ;
#6624 = ADVANCED_FACE ( 'NONE', ( #7651 ), #2086, .F. ) ;
#6625 = CARTESIAN_POINT ( 'NONE',  ( -13.50000000000000000, -43.00000000000000000, -137.0552959530000123 ) ) ;
#6626 = LINE ( 'NONE', #15556, #9834 ) ;
#6627 = ORIENTED_EDGE ( 'NONE', *, *, #19817, .T. ) ;
#6628 = EDGE_CURVE ( 'NONE', #3906, #21536, #9419, .T. ) ;
#6629 = EDGE_CURVE ( 'NONE', #2237, #20657, #411, .T. ) ;
#6630 = DIRECTION ( 'NONE',  ( 1.000000000000000000, 0.000000000000000000, -2.775557561562891351E-14 ) ) ;
#6631 = ORIENTED_EDGE ( 'NONE', *, *, #17358, .F. ) ;
#6632 = CARTESIAN_POINT ( 'NONE',  ( 23.78818517497548513, -17.51387386322154072, -148.5552959529998418 ) ) ;
#6633 = PLANE ( 'NONE',  #15809 ) ;
#6634 = EDGE_CURVE ( 'NONE', #21412, #12329, #2322, .T. ) ;
#6635 = VERTEX_POINT ( 'NONE', #14922 ) ;
#6636 = CARTESIAN_POINT ( 'NONE',  ( -20.28536656041405450, 36.96856293252766790, -139.5160734784155636 ) ) ;
#6637 = CARTESIAN_POINT ( 'NONE',  ( 3.999999999879999546, -3.500000000000000000, -135.4552959529999896 ) ) ;
#6638 = VERTEX_POINT ( 'NONE', #13238 ) ;
#6639 = CARTESIAN_POINT ( 'NONE',  ( -14.78397831697835763, 38.75612598996944769, -139.9015999578828655 ) ) ;
#6640 = CARTESIAN_POINT ( 'NONE',  ( -25.30581943868956429, 34.34500769354227856, -147.8257434426395207 ) ) ;
#6641 = EDGE_LOOP ( 'NONE', ( #542, #5257, #4230, #10402 ) ) ;
#6642 = FILL_AREA_STYLE_COLOUR ( '', #16827 ) ;
#6643 = ORIENTED_EDGE ( 'NONE', *, *, #12079, .T. ) ;
#6644 = CARTESIAN_POINT ( 'NONE',  ( -11.86981903010000039, 40.35288497620000214, -142.1893091610000113 ) ) ;
#6645 = FACE_OUTER_BOUND ( 'NONE', #10270, .T. ) ;
#6646 = ORIENTED_EDGE ( 'NONE', *, *, #7785, .F. ) ;
#6647 = DIRECTION ( 'NONE',  ( -0.1435602414469281940, -0.9896415801065048257, 3.849849731938073961E-13 ) ) ;
#6648 = LINE ( 'NONE', #1320, #9806 ) ;
#6649 = CARTESIAN_POINT ( 'NONE',  ( -25.86630785129999666, -50.50000000000000000, -136.5552959530000123 ) ) ;
#6650 = AXIS2_PLACEMENT_3D ( 'NONE', #15116, #21192, #10092 ) ;
#6651 = ORIENTED_EDGE ( 'NONE', *, *, #2842, .T. ) ;
#6652 = FACE_OUTER_BOUND ( 'NONE', #8019, .T. ) ;
#6653 = EDGE_CURVE ( 'NONE', #19799, #6863, #9304, .T. ) ;
#6654 = LINE ( 'NONE', #19272, #21479 ) ;
#6655 = EDGE_CURVE ( 'NONE', #8318, #11000, #9548, .T. ) ;
#6656 = CARTESIAN_POINT ( 'NONE',  ( -15.14817811019070248, 37.92142832241574268, -148.5963073275012221 ) ) ;
#6657 = FACE_OUTER_BOUND ( 'NONE', #13549, .T. ) ;
#6658 = VERTEX_POINT ( 'NONE', #16468 ) ;
#6659 = CARTESIAN_POINT ( 'NONE',  ( 13.13369214859999978, -50.50000000000000000, -137.0552959530000123 ) ) ;
#6660 = LINE ( 'NONE', #9142, #4406 ) ;
#6661 = PLANE ( 'NONE',  #10645 ) ;
#6662 = CARTESIAN_POINT ( 'NONE',  ( -9.056357402059999728, -12.43025388040000045, -147.5552959529999839 ) ) ;
#6663 = LINE ( 'NONE', #13927, #17161 ) ;
#6664 = CARTESIAN_POINT ( 'NONE',  ( -12.50000000000000000, 48.50000000000000000, -136.5552959530000123 ) ) ;
#6665 = VECTOR ( 'NONE', #9772, 999.9999999999998863 ) ;
#6666 = AXIS2_PLACEMENT_3D ( 'NONE', #15300, #793, #11470 ) ;
#6667 = VERTEX_POINT ( 'NONE', #4088 ) ;
#6668 = FACE_OUTER_BOUND ( 'NONE', #19252, .T. ) ;
#6669 = DIRECTION ( 'NONE',  ( -1.000000000000000000, 0.000000000000000000, 0.000000000000000000 ) ) ;
#6670 = CARTESIAN_POINT ( 'NONE',  ( -5.480550747629762576, 36.94526453639895180, -140.5641745855584190 ) ) ;
#6671 = CARTESIAN_POINT ( 'NONE',  ( 22.01137100460000084, -15.39610142400000115, -147.5552959529999839 ) ) ;
#6672 = DIRECTION ( 'NONE',  ( -0.000000000000000000, 1.000000000000000000, 0.000000000000000000 ) ) ;
#6673 = ORIENTED_EDGE ( 'NONE', *, *, #16917, .T. ) ;
#6674 = CARTESIAN_POINT ( 'NONE',  ( -10.41700570847820551, 37.07221587398769458, -140.3414633426675380 ) ) ;
#6675 = LINE ( 'NONE', #13937, #15303 ) ;
#6676 = CARTESIAN_POINT ( 'NONE',  ( -25.73504040789999792, 33.16200571349999393, -143.7184748760000161 ) ) ;
#6677 = ORIENTED_EDGE ( 'NONE', *, *, #11955, .F. ) ;
#6679 = CARTESIAN_POINT ( 'NONE',  ( -29.17292895941881881, 34.79208654433700332, -141.0602999640023256 ) ) ;
#6678 = CIRCLE ( 'NONE', #14673, 1.500000000000001332 ) ;
#6680 = VECTOR ( 'NONE', #16467, 1000.000000000000000 ) ;
#6681 = CARTESIAN_POINT ( 'NONE',  ( 1.693247834384973283, -17.47463886119383503, -146.5552959530003250 ) ) ;
#6682 = ORIENTED_EDGE ( 'NONE', *, *, #18429, .T. ) ;
#6683 = EDGE_CURVE ( 'NONE', #20086, #17769, #532, .T. ) ;
#6684 = CARTESIAN_POINT ( 'NONE',  ( -22.96991264454272752, 40.42754630402341576, -142.1998910728711962 ) ) ;
#6685 = EDGE_CURVE ( 'NONE', #22568, #14539, #65, .T. ) ;
#6686 = CARTESIAN_POINT ( 'NONE',  ( 32.00000000000000000, 32.96379895120000469, -137.0552959530000123 ) ) ;
#6687 = CARTESIAN_POINT ( 'NONE',  ( 1.000000000140000012, 41.50000000000000000, -147.5552959529999839 ) ) ;
#6688 = CARTESIAN_POINT ( 'NONE',  ( 8.108818582516752471, 38.44893568608949863, -142.0179551230363870 ) ) ;
#6689 = ORIENTED_EDGE ( 'NONE', *, *, #17328, .F. ) ;
#6690 = CARTESIAN_POINT ( 'NONE',  ( -10.05941948556869292, 36.05287800962796751, -148.5984116296196476 ) ) ;
#6691 = EDGE_CURVE ( 'NONE', #6609, #4038, #4485, .T. ) ;
#6692 = CARTESIAN_POINT ( 'NONE',  ( 4.084326842523585910, 27.61765588495835644, -150.0552959529999839 ) ) ;
#6693 = LINE ( 'NONE', #5140, #2975 ) ;
#6694 = CARTESIAN_POINT ( 'NONE',  ( -2.491922975426976272, -28.49278486398841181, -144.5552959529864552 ) ) ;
#6695 = ORIENTED_EDGE ( 'NONE', *, *, #9122, .T. ) ;
#6696 =( LENGTH_UNIT ( ) NAMED_UNIT ( * ) SI_UNIT ( .MILLI., .METRE. ) );
#6697 = VERTEX_POINT ( 'NONE', #175 ) ;
#6698 = VECTOR ( 'NONE', #19460, 1000.000000000000000 ) ;
#6699 = CARTESIAN_POINT ( 'NONE',  ( -6.486810516462077736, 36.30202410411560976, -147.3923230133318043 ) ) ;
#6700 = CARTESIAN_POINT ( 'NONE',  ( -29.94412816099999830, 41.23953273989999957, -145.7122098469999969 ) ) ;
#6701 = LINE ( 'NONE', #21116, #17253 ) ;
#6702 = EDGE_CURVE ( 'NONE', #16262, #6658, #21934, .T. ) ;
#6703 = EDGE_LOOP ( 'NONE', ( #14346, #15084, #13232, #8890 ) ) ;
#6704 = FACE_OUTER_BOUND ( 'NONE', #183, .T. ) ;
#6705 = CARTESIAN_POINT ( 'NONE',  ( -9.347107914279998653, -17.32706600430000066, -144.5552959529999839 ) ) ;
#6706 = ORIENTED_EDGE ( 'NONE', *, *, #19289, .T. ) ;
#6707 = FACE_OUTER_BOUND ( 'NONE', #2578, .T. ) ;
#6708 = CARTESIAN_POINT ( 'NONE',  ( -18.58114728243741709, 40.89578867383085736, -146.1569481741396999 ) ) ;
#6709 = DIRECTION ( 'NONE',  ( 1.000000000000000000, 0.000000000000000000, -2.258609965721802837E-12 ) ) ;
#6710 = DIRECTION ( 'NONE',  ( 1.000000000000000000, 0.000000000000000000, -4.510281037539699253E-12 ) ) ;
#6711 = ADVANCED_FACE ( 'NONE', ( #5522 ), #13122, .F. ) ;
#6712 = CARTESIAN_POINT ( 'NONE',  ( -7.081915218180246718, 37.06683495600067602, -147.7519347211649006 ) ) ;
#6713 = VECTOR ( 'NONE', #10915, 1000.000000000000000 ) ;
#6714 = DIRECTION ( 'NONE',  ( -4.510774274160000731E-12, 1.321907670990000086E-13, -1.000000000000000000 ) ) ;
#6715 = CARTESIAN_POINT ( 'NONE',  ( 23.93638409349999918, -31.59322175579999836, -144.5552959529999839 ) ) ;
#6716 = EDGE_CURVE ( 'NONE', #5950, #4170, #20171, .T. ) ;
#6717 = CARTESIAN_POINT ( 'NONE',  ( 19.00000000000000000, 39.50000000000000000, -150.0552959529999839 ) ) ;
#6718 = EDGE_LOOP ( 'NONE', ( #17930, #7128, #7658, #14718, #588 ) ) ;
#6719 = FACE_OUTER_BOUND ( 'NONE', #3345, .T. ) ;
#6721 = ORIENTED_EDGE ( 'NONE', *, *, #10981, .F. ) ;
#6720 = PRODUCT_DEFINITION ( 'UNKNOWN', '', #6975, #18031 ) ;
#6722 = FILL_AREA_STYLE_COLOUR ( '', #22134 ) ;
#6723 = EDGE_CURVE ( 'NONE', #6638, #21976, #271, .T. ) ;
#6724 = ORIENTED_EDGE ( 'NONE', *, *, #15661, .T. ) ;
#6725 = CARTESIAN_POINT ( 'NONE',  ( 3.611688725869999975E-11, 21.50000000000000000, -136.0552959530000123 ) ) ;
#6726 = DIRECTION ( 'NONE',  ( -0.1146332952500066227, -0.9934078757590583120, -9.947598300640582187E-14 ) ) ;
#6727 = ORIENTED_EDGE ( 'NONE', *, *, #90, .F. ) ;
#6728 = AXIS2_PLACEMENT_3D ( 'NONE', #18397, #21866, #18750 ) ;
#6729 = VERTEX_POINT ( 'NONE', #4679 ) ;
#6730 = LINE ( 'NONE', #10409, #1139 ) ;
#6731 = CIRCLE ( 'NONE', #2939, 3.000000000000000888 ) ;
#6732 = DIRECTION ( 'NONE',  ( 4.430318231639999944E-12, -6.100259101500000139E-13, 1.000000000000000000 ) ) ;
#6733 = DIRECTION ( 'NONE',  ( -0.9748402797454081004, 0.2229045288590935092, 4.454830202381862158E-12 ) ) ;
#6734 = CARTESIAN_POINT ( 'NONE',  ( 16.87269471589999981, -31.91616505980000085, -144.0552959529999839 ) ) ;
#6735 = EDGE_CURVE ( 'NONE', #12862, #8946, #7107, .T. ) ;
#6736 = ORIENTED_EDGE ( 'NONE', *, *, #11945, .T. ) ;
#6737 = DIRECTION ( 'NONE',  ( 1.000000000000000000, 0.000000000000000000, -8.955190032050000935E-12 ) ) ;
#6738 = CARTESIAN_POINT ( 'NONE',  ( -18.35824191589999899, -1.500000000000000000, -142.9407682190000060 ) ) ;
#6739 = CARTESIAN_POINT ( 'NONE',  ( 31.50000000000000000, 40.03620104880000241, -136.0552959530000123 ) ) ;
#6740 = EDGE_CURVE ( 'NONE', #3396, #21050, #22761, .T. ) ;
#6741 = VERTEX_POINT ( 'NONE', #20632 ) ;
#6742 = AXIS2_PLACEMENT_3D ( 'NONE', #22612, #7969, #4526 ) ;
#6743 = CARTESIAN_POINT ( 'NONE',  ( 1.393351898023278412, -20.95564341188169522, -143.5552959529982218 ) ) ;
#6744 = VECTOR ( 'NONE', #21311, 1000.000000000000000 ) ;
#6745 = ORIENTED_EDGE ( 'NONE', *, *, #17409, .F. ) ;
#6746 = CARTESIAN_POINT ( 'NONE',  ( -20.36280570459999595, 40.92149091569999797, -144.5882336180000038 ) ) ;
#6747 = PLANE ( 'NONE',  #21906 ) ;
#6748 = VERTEX_POINT ( 'NONE', #6574 ) ;
#6749 = DIRECTION ( 'NONE',  ( 0.000000000000000000, -1.000000000000000000, 0.000000000000000000 ) ) ;
#6750 = LINE ( 'NONE', #10541, #11087 ) ;
#6751 = ORIENTED_EDGE ( 'NONE', *, *, #18061, .F. ) ;
#6752 = CARTESIAN_POINT ( 'NONE',  ( -14.56152959349201481, 39.73338309561681569, -140.2290243436648609 ) ) ;
#6753 = EDGE_CURVE ( 'NONE', #5050, #19419, #8729, .T. ) ;
#6754 = CARTESIAN_POINT ( 'NONE',  ( -26.09056442780078910, 32.98054588081366489, -141.8362709652814715 ) ) ;
#6755 = ORIENTED_EDGE ( 'NONE', *, *, #16548, .F. ) ;
#6756 = VERTEX_POINT ( 'NONE', #18730 ) ;
#6757 = LINE ( 'NONE', #17712, #8322 ) ;
#6758 = CARTESIAN_POINT ( 'NONE',  ( 10.68320006080000084, -20.50000000000000000, -150.0552959529999839 ) ) ;
#6759 = ORIENTED_EDGE ( 'NONE', *, *, #5728, .T. ) ;
#6760 = DIRECTION ( 'NONE',  ( 2.262447131730000305E-12, 0.000000000000000000, 1.000000000000000000 ) ) ;
#6761 = VECTOR ( 'NONE', #42, 1000.000000000000000 ) ;
#6762 = EDGE_CURVE ( 'NONE', #20510, #20921, #18452, .T. ) ;
#6763 = CARTESIAN_POINT ( 'NONE',  ( 25.96278831649999930, -46.03148680910000223, -136.0552959530000123 ) ) ;
#6764 = EDGE_CURVE ( 'NONE', #9544, #16508, #17741, .T. ) ;
#6765 = VECTOR ( 'NONE', #12448, 1000.000000000000000 ) ;
#6766 = LINE ( 'NONE', #4643, #714 ) ;
#6767 = ADVANCED_FACE ( 'NONE', ( #17402 ), #2783, .F. ) ;
#6768 = EDGE_CURVE ( 'NONE', #17007, #21283, #887, .T. ) ;
#6769 = ORIENTED_EDGE ( 'NONE', *, *, #17380, .T. ) ;
#6770 =( BOUNDED_CURVE ( )  B_SPLINE_CURVE ( 5, ( #4107, #18050, #7674, #18396, #11122, #21970 ),
 .UNSPECIFIED., .F., .F. ) 
 B_SPLINE_CURVE_WITH_KNOTS ( ( 6, 6 ),
 ( 0.000000000000000000, 1.570796326683616906 ),
 .UNSPECIFIED. ) 
 CURVE ( )  GEOMETRIC_REPRESENTATION_ITEM ( )  RATIONAL_B_SPLINE_CURVE ( ( 1.000000000000000000, 0.6000000000283634005, 0.4000000000283634449, 0.3000000000212725837, 0.2500000000141817114, 0.2499999999999999722 ) ) 
 REPRESENTATION_ITEM ( '' )  );
#6771 = DIRECTION ( 'NONE',  ( 1.000000000000000000, 0.000000000000000000, -2.257453483404485639E-12 ) ) ;
#6772 = CARTESIAN_POINT ( 'NONE',  ( -8.770737564319999180, -11.35481373070000011, -144.5552959529999839 ) ) ;
#6773 = CARTESIAN_POINT ( 'NONE',  ( -14.93328160134642957, 36.92972691758554049, -148.3740393307390661 ) ) ;
#6774 = LINE ( 'NONE', #4878, #4923 ) ;
#6775 = ORIENTED_EDGE ( 'NONE', *, *, #6764, .T. ) ;
#6776 = PLANE ( 'NONE',  #4087 ) ;
#6777 = CARTESIAN_POINT ( 'NONE',  ( -18.35824191589999899, -34.50000000000000000, -148.1907682189999775 ) ) ;
#6778 = VECTOR ( 'NONE', #2655, 1000.000000000000000 ) ;
#6779 = PLANE ( 'NONE',  #23185 ) ;
#6780 = VECTOR ( 'NONE', #2478, 1000.000000000000000 ) ;
#6781 = DIRECTION ( 'NONE',  ( -0.7071067811865475727, 0.7071067811865475727, 0.000000000000000000 ) ) ;
#6782 = DIRECTION ( 'NONE',  ( -2.256988247010000033E-12, 0.000000000000000000, 1.000000000000000000 ) ) ;
#6783 = CARTESIAN_POINT ( 'NONE',  ( -4.021770264099999714, -29.17051924670000318, -143.0552959529999839 ) ) ;
#6784 = AXIS2_PLACEMENT_3D ( 'NONE', #243, #9719, #4385 ) ;
#6785 = ORIENTED_EDGE ( 'NONE', *, *, #15697, .T. ) ;
#6786 = CARTESIAN_POINT ( 'NONE',  ( -17.22605506639999717, 36.97564272059999979, -139.5994799229999899 ) ) ;
#6787 = VECTOR ( 'NONE', #13060, 1000.000000000000000 ) ;
#6788 = FACE_OUTER_BOUND ( 'NONE', #13904, .T. ) ;
#6789 = CARTESIAN_POINT ( 'NONE',  ( 21.44117969379999877, -21.36894679869999791, -147.5552959529999839 ) ) ;
#6790 = CARTESIAN_POINT ( 'NONE',  ( 7.200097415480000151, -13.39991276200000136, -144.5552959529999839 ) ) ;
#6791 = CARTESIAN_POINT ( 'NONE',  ( 12.81474735470000148, -17.96536370379999781, -144.5552959529999839 ) ) ;
#6792 = VERTEX_POINT ( 'NONE', #9658 ) ;
#6793 = CARTESIAN_POINT ( 'NONE',  ( -18.07392865170000107, -34.50000000000000000, -147.3157682190000060 ) ) ;
#6794 = ADVANCED_FACE ( 'NONE', ( #10010 ), #20744, .T. ) ;
#6795 = DIRECTION ( 'NONE',  ( -4.510170015240000199E-12, 1.314504061159999897E-13, -1.000000000000000000 ) ) ;
#6796 = ORIENTED_EDGE ( 'NONE', *, *, #1963, .F. ) ;
#6797 = VECTOR ( 'NONE', #14450, 1000.000000000000000 ) ;
#6798 = VECTOR ( 'NONE', #8112, 1000.000000000000000 ) ;
#6799 = DIRECTION ( 'NONE',  ( 0.000000000000000000, 0.000000000000000000, -1.000000000000000000 ) ) ;
#6800 = PLANE ( 'NONE',  #20891 ) ;
#6801 = ORIENTED_EDGE ( 'NONE', *, *, #21508, .T. ) ;
#6802 = VECTOR ( 'NONE', #5015, 1000.000000000000000 ) ;
#6803 = CARTESIAN_POINT ( 'NONE',  ( -34.61111111099999960, 45.00000000000000000, -140.5552959529999839 ) ) ;
#6804 = CARTESIAN_POINT ( 'NONE',  ( -30.49999999990000177, 45.00000000000000000, -147.5552959529999839 ) ) ;
#6805 = CIRCLE ( 'NONE', #17837, 9.999999999999998224 ) ;
#6806 = CYLINDRICAL_SURFACE ( 'NONE', #14344, 2.500000000000002220 ) ;
#6807 = CARTESIAN_POINT ( 'NONE',  ( 7.571119092374880566, 38.17802949123974798, -141.8499009779202140 ) ) ;
#6808 = ORIENTED_EDGE ( 'NONE', *, *, #16973, .F. ) ;
#6809 = CARTESIAN_POINT ( 'NONE',  ( -4.683324139160000676, 37.83302525630000446, -140.3020749749999823 ) ) ;
#6810 = CARTESIAN_POINT ( 'NONE',  ( -1.000000000000000222, 20.99262443222763608, -150.0552959530000123 ) ) ;
#6811 = CARTESIAN_POINT ( 'NONE',  ( -6.477935707790000386, -19.20465386649999928, -146.5552959529999839 ) ) ;
#6812 = LINE ( 'NONE', #6133, #4994 ) ;
#6813 = ORIENTED_EDGE ( 'NONE', *, *, #1107, .T. ) ;
#6814 = LINE ( 'NONE', #8118, #15240 ) ;
#6815 = VECTOR ( 'NONE', #8572, 999.9999999999998863 ) ;
#6816 = CIRCLE ( 'NONE', #3409, 2.500000000000000444 ) ;
#6817 = VERTEX_POINT ( 'NONE', #8354 ) ;
#6818 = CARTESIAN_POINT ( 'NONE',  ( -7.593515551632238569, 36.30629168799562478, -140.6345953673100553 ) ) ;
#6819 = CARTESIAN_POINT ( 'NONE',  ( -6.705189174439999178, 39.56570632409999888, -147.4373625599999968 ) ) ;
#6820 = DIRECTION ( 'NONE',  ( 0.000000000000000000, 1.000000000000000000, 0.000000000000000000 ) ) ;
#6821 = VECTOR ( 'NONE', #16019, 1000.000000000000227 ) ;
#6822 = ORIENTED_EDGE ( 'NONE', *, *, #8631, .F. ) ;
#6823 = EDGE_CURVE ( 'NONE', #7697, #19038, #16931, .T. ) ;
#6824 = CIRCLE ( 'NONE', #11749, 2.499999999999998668 ) ;
#6825 = CARTESIAN_POINT ( 'NONE',  ( 5.792747474879999636, -16.92794981449999980, -145.5552959529999839 ) ) ;
#6826 = VECTOR ( 'NONE', #22603, 1000.000000000000000 ) ;
#6827 = LINE ( 'NONE', #3154, #6836 ) ;
#6828 = EDGE_LOOP ( 'NONE', ( #18220, #6296, #16409, #20832, #3572, #20707, #7912, #1772, #20208, #19025, #13112, #9318 ) ) ;
#6829 = DIRECTION ( 'NONE',  ( 0.000000000000000000, -4.148443855749999753E-27, -1.000000000000000000 ) ) ;
#6830 = CARTESIAN_POINT ( 'NONE',  ( -19.14899212251805949, 37.07484167171462275, -147.8220480108583956 ) ) ;
#6831 = CARTESIAN_POINT ( 'NONE',  ( 7.558347240409999834, -12.62842008530000015, -147.5552959529999839 ) ) ;
#6832 = DIRECTION ( 'NONE',  ( 0.000000000000000000, 0.000000000000000000, 1.000000000000000000 ) ) ;
#6833 = LINE ( 'NONE', #17780, #15412 ) ;
#6834 = CARTESIAN_POINT ( 'NONE',  ( -17.22605506639999717, 36.97564272059999979, -139.5994799229999899 ) ) ;
#6835 = FACE_OUTER_BOUND ( 'NONE', #2247, .T. ) ;
#6836 = VECTOR ( 'NONE', #10383, 1000.000000000000000 ) ;
#6837 = CARTESIAN_POINT ( 'NONE',  ( 31.50000000010000178, 40.03620104870000063, -143.0552959529999839 ) ) ;
#6838 = AXIS2_PLACEMENT_3D ( 'NONE', #20762, #13735, #1016 ) ;
#6839 = AXIS2_PLACEMENT_3D ( 'NONE', #325, #21984, #9238 ) ;
#6840 = VECTOR ( 'NONE', #16053, 1000.000000000000000 ) ;
#6841 = EDGE_LOOP ( 'NONE', ( #15409, #2575, #247, #10506 ) ) ;
#6842 = CARTESIAN_POINT ( 'NONE',  ( -29.13601448249999848, 36.98639052360000079, -140.5419328609999923 ) ) ;
#6843 = UNCERTAINTY_MEASURE_WITH_UNIT (LENGTH_MEASURE( 1.000000000000000082E-05 ), #16105, 'distance_accuracy_value', 'NONE');
#6844 = ORIENTED_EDGE ( 'NONE', *, *, #2138, .T. ) ;
#6845 = ORIENTED_EDGE ( 'NONE', *, *, #470, .F. ) ;
#6846 = CARTESIAN_POINT ( 'NONE',  ( -16.16658683015744202, 37.07694188522086876, -148.2333767340493011 ) ) ;
#6847 = CARTESIAN_POINT ( 'NONE',  ( -12.50000000000000000, 25.50000000000000000, -150.5552959529999839 ) ) ;
#6848 = EDGE_LOOP ( 'NONE', ( #12403, #8508, #18544, #10206 ) ) ;
#6849 = ORIENTED_EDGE ( 'NONE', *, *, #14812, .F. ) ;
#6850 = EDGE_CURVE ( 'NONE', #16441, #12024, #13362, .T. ) ;
#6851 = CARTESIAN_POINT ( 'NONE',  ( -4.499932713042313459, 22.10251055751543348, -150.0552959529999839 ) ) ;
#6852 = CARTESIAN_POINT ( 'NONE',  ( 1.000000000160000013, 36.50000000000000000, -139.5552959529999839 ) ) ;
#6853 = DIRECTION ( 'NONE',  ( 1.000000000000000000, 0.000000000000000000, -4.430318231639999944E-12 ) ) ;
#6854 = EDGE_CURVE ( 'NONE', #9593, #20938, #1596, .T. ) ;
#6855 = DIRECTION ( 'NONE',  ( 2.256861364460000137E-12, 0.000000000000000000, 1.000000000000000000 ) ) ;
#6856 = CIRCLE ( 'NONE', #1942, 1.500000000000001332 ) ;
#6857 = STYLED_ITEM ( 'NONE', ( #13113 ), #11538 ) ;
#6858 = CARTESIAN_POINT ( 'NONE',  ( -8.411849887919201407, 36.09637009089656345, -140.1322081666141912 ) ) ;
#6859 = ORIENTED_EDGE ( 'NONE', *, *, #17213, .F. ) ;
#6860 = CARTESIAN_POINT ( 'NONE',  ( 9.722460972908612220, 36.13064952216455339, -141.7113041811295773 ) ) ;
#6861 = CYLINDRICAL_SURFACE ( 'NONE', #6040, 2.500000000000001776 ) ;
#6862 = CARTESIAN_POINT ( 'NONE',  ( 1.172620240290000115, -63.19354141059999108, -145.5552959529999839 ) ) ;
#6863 = VERTEX_POINT ( 'NONE', #13947 ) ;
#6864 = LINE ( 'NONE', #14707, #823 ) ;
#6865 = VERTEX_POINT ( 'NONE', #10258 ) ;
#6866 = DIRECTION ( 'NONE',  ( 0.04459224566432164888, 0.9990052710704848682, -8.219575497233998330E-13 ) ) ;
#6867 = DIRECTION ( 'NONE',  ( 8.645353842254780479E-13, 0.000000000000000000, -1.000000000000000000 ) ) ;
#6868 = VECTOR ( 'NONE', #5144, 1000.000000000000000 ) ;
#6869 = EDGE_CURVE ( 'NONE', #20874, #9011, #12506, .T. ) ;
#6870 = VERTEX_POINT ( 'NONE', #8692 ) ;
#6871 = CARTESIAN_POINT ( 'NONE',  ( -17.08727435560000174, -34.50000000000000000, -147.1525923079999814 ) ) ;
#6872 = CARTESIAN_POINT ( 'NONE',  ( 26.12135916506278122, -22.01085694111269220, -150.0552959529999839 ) ) ;
#6873 = VERTEX_POINT ( 'NONE', #15973 ) ;
#6874 = CARTESIAN_POINT ( 'NONE',  ( -21.84190187641215886, 35.02767429215685269, -148.4596182608835875 ) ) ;
#6875 = CARTESIAN_POINT ( 'NONE',  ( -12.50000000000000000, 48.50000000000000000, -151.0552959529999839 ) ) ;
#6876 = ORIENTED_EDGE ( 'NONE', *, *, #104, .F. ) ;
#6877 = DIRECTION ( 'NONE',  ( 0.000000000000000000, 0.000000000000000000, 1.000000000000000000 ) ) ;
#6878 = ORIENTED_EDGE ( 'NONE', *, *, #19836, .T. ) ;
#6879 = DIRECTION ( 'NONE',  ( 1.000000000000000000, 0.000000000000000000, -2.257453483404485639E-12 ) ) ;
#6880 = DIRECTION ( 'NONE',  ( 1.000000000000000000, 0.000000000000000000, -8.954760363766765626E-12 ) ) ;
#6881 = ORIENTED_EDGE ( 'NONE', *, *, #16129, .F. ) ;
#6882 = DIRECTION ( 'NONE',  ( 1.211690350419999855E-27, 2.765629237170000203E-27, -1.000000000000000000 ) ) ;
#6883 = LINE ( 'NONE', #17960, #2253 ) ;
#6884 = ORIENTED_EDGE ( 'NONE', *, *, #605, .T. ) ;
#6885 = DIRECTION ( 'NONE',  ( 2.255973186040000320E-12, 0.000000000000000000, 1.000000000000000000 ) ) ;
#6886 = VECTOR ( 'NONE', #6986, 1000.000000000000000 ) ;
#6887 = CLOSED_SHELL ( 'NONE', ( #23245, #16871, #1713, #13548, #19346, #10841, #20769, #19401, #7857, #2617, #10509, #19594, #9099, #19097, #15877, #1845, #20291, #4876, #7964 ) ) ;
#6888 = AXIS2_PLACEMENT_3D ( 'NONE', #6315, #15366, #2766 ) ;
#6889 = EDGE_CURVE ( 'NONE', #21170, #7540, #2180, .T. ) ;
#6890 = ORIENTED_EDGE ( 'NONE', *, *, #16204, .F. ) ;
#6891 = CARTESIAN_POINT ( 'NONE',  ( 0.1832000607640000001, -6.500000000000000000, -149.3052959529999839 ) ) ;
#6892 = FACE_BOUND ( 'NONE', #10820, .T. ) ;
#6893 = CARTESIAN_POINT ( 'NONE',  ( -14.35880640235731143, 41.60548537699954608, -143.5801344958343861 ) ) ;
#6894 = DIRECTION ( 'NONE',  ( 1.000000000000000000, 0.000000000000000000, -8.953948693601887499E-12 ) ) ;
#6895 = EDGE_LOOP ( 'NONE', ( #9583, #207, #23122, #6435, #8029, #12422 ) ) ;
#6896 = DIRECTION ( 'NONE',  ( 0.000000000000000000, 0.8775825618903703162, 0.4794255386042076128 ) ) ;
#6897 = LINE ( 'NONE', #10101, #4772 ) ;
#6898 = ADVANCED_FACE ( 'NONE', ( #22997 ), #14189, .T. ) ;
#6899 = FACE_OUTER_BOUND ( 'NONE', #14811, .T. ) ;
#6900 = DIRECTION ( 'NONE',  ( 0.000000000000000000, -4.148443855749999753E-27, -1.000000000000000000 ) ) ;
#6901 = DIRECTION ( 'NONE',  ( 1.000000000000000000, 0.000000000000000000, 0.000000000000000000 ) ) ;
#6902 = PLANE ( 'NONE',  #6406 ) ;
#6903 = EDGE_CURVE ( 'NONE', #7002, #17964, #1246, .T. ) ;
#6904 = AXIS2_PLACEMENT_3D ( 'NONE', #10569, #5479, #17731 ) ;
#6905 = ORIENTED_EDGE ( 'NONE', *, *, #1982, .F. ) ;
#6906 = VECTOR ( 'NONE', #5298, 1000.000000000000000 ) ;
#6907 = DIRECTION ( 'NONE',  ( 2.257171095940000041E-12, 1.003664318210000046E-28, 1.000000000000000000 ) ) ;
#6908 = EDGE_CURVE ( 'NONE', #20527, #4267, #16211, .T. ) ;
#6909 = DIRECTION ( 'NONE',  ( 1.000000000000000000, 0.000000000000000000, 2.506439500389999993E-12 ) ) ;
#6910 = DIRECTION ( 'NONE',  ( -0.1146332952500066227, -0.9934078757590583120, -1.023181539490060155E-13 ) ) ;
#6911 = EDGE_CURVE ( 'NONE', #14227, #2700, #21554, .T. ) ;
#6912 = CARTESIAN_POINT ( 'NONE',  ( -5.345822467930000599, 40.94956462150000220, -144.4907973060000188 ) ) ;
#6913 = FACE_OUTER_BOUND ( 'NONE', #20084, .T. ) ;
#6914 = LINE ( 'NONE', #10816, #19169 ) ;
#6915 = ORIENTED_EDGE ( 'NONE', *, *, #15793, .F. ) ;
#6916 = CYLINDRICAL_SURFACE ( 'NONE', #9204, 1.500000000000001332 ) ;
#6917 = DIRECTION ( 'NONE',  ( -1.000000000000000000, 0.000000000000000000, 2.257495777610000006E-12 ) ) ;
#6918 = ORIENTED_EDGE ( 'NONE', *, *, #2515, .F. ) ;
#6919 = SHAPE_REPRESENTATION ( 'Cover Plate', ( #5025 ), #1616 ) ;
#6920 = AXIS2_PLACEMENT_3D ( 'NONE', #11163, #21904, #11051 ) ;
#6921 = CIRCLE ( 'NONE', #6158, 2.999999999999999112 ) ;
#6922 = LINE ( 'NONE', #14298, #18976 ) ;
#6923 = EDGE_LOOP ( 'NONE', ( #17541, #21523, #19105, #5321 ) ) ;
#6924 = EDGE_CURVE ( 'NONE', #16352, #11025, #1052, .T. ) ;
#6925 = CIRCLE ( 'NONE', #21000, 0.7500000000000006661 ) ;
#6926 = CARTESIAN_POINT ( 'NONE',  ( -13.50000000000000000, -43.00000000000000000, -145.5552959529999839 ) ) ;
#6927 = CARTESIAN_POINT ( 'NONE',  ( -6.366307851350000213, 50.50000000000000000, -137.0552959530000123 ) ) ;
#6928 = CARTESIAN_POINT ( 'NONE',  ( 22.42591623494620023, -15.34961090601114542, -144.5552959529997281 ) ) ;
#6929 = CARTESIAN_POINT ( 'NONE',  ( 6.999997771067969943, 36.90428341750195784, -141.5552923337224058 ) ) ;
#6930 = ORIENTED_EDGE ( 'NONE', *, *, #3076, .F. ) ;
#6931 = CARTESIAN_POINT ( 'NONE',  ( -11.49975391485736509, 36.06355900336099296, -139.6950141698461891 ) ) ;
#6932 = CARTESIAN_POINT ( 'NONE',  ( -17.89449577229611776, 36.92509720026576758, -147.9522036891032428 ) ) ;
#6933 = EDGE_CURVE ( 'NONE', #8763, #15072, #1450, .T. ) ;
#6934 = CARTESIAN_POINT ( 'NONE',  ( 22.50000000000000000, 33.50000000000000000, -136.0552959530000123 ) ) ;
#6935 = CARTESIAN_POINT ( 'NONE',  ( 8.976561295290075293, -35.78342539458139271, -136.0552959530202770 ) ) ;
#6936 = VERTEX_POINT ( 'NONE', #12385 ) ;
#6937 = EDGE_CURVE ( 'NONE', #16896, #15538, #1350, .T. ) ;
#6938 = PLANE ( 'NONE',  #19812 ) ;
#6939 = ORIENTED_EDGE ( 'NONE', *, *, #9178, .F. ) ;
#6940 = CARTESIAN_POINT ( 'NONE',  ( -7.366919058817297028, 34.86075545065775572, -147.1984919235340783 ) ) ;
#6941 = CARTESIAN_POINT ( 'NONE',  ( -23.96729089089999931, 37.81249143149999981, -148.2640374880000138 ) ) ;
#6942 = DIRECTION ( 'NONE',  ( 0.1435602414469281940, 0.9896415801065048257, -3.836930773098079160E-13 ) ) ;
#6943 = VECTOR ( 'NONE', #19420, 1000.000000000000000 ) ;
#6944 = EDGE_LOOP ( 'NONE', ( #5453, #20053, #10536, #3422 ) ) ;
#6945 = CARTESIAN_POINT ( 'NONE',  ( -5.195035615602224155, 37.68216517631442741, -140.7224638479279690 ) ) ;
#6946 = CARTESIAN_POINT ( 'NONE',  ( -3.499999999959999997, 40.00000000000000000, -136.0552959530000123 ) ) ;
#6947 = ORIENTED_EDGE ( 'NONE', *, *, #18138, .F. ) ;
#6948 = DIRECTION ( 'NONE',  ( 0.9953753789357124848, -0.09606172499277225441, -7.355811845627870223E-14 ) ) ;
#6949 = FACE_OUTER_BOUND ( 'NONE', #17833, .T. ) ;
#6950 = DIRECTION ( 'NONE',  ( 0.000000000000000000, 4.426606872070000353E-37, -1.000000000000000000 ) ) ;
#6951 = PLANE ( 'NONE',  #23169 ) ;
#6952 = CARTESIAN_POINT ( 'NONE',  ( -32.50000000000000000, -64.50000000000000000, -144.0552959529999839 ) ) ;
#6953 = CARTESIAN_POINT ( 'NONE',  ( -2.100773033209999863, -15.22510554480000167, -145.5552959529999839 ) ) ;
#6954 = APPLICATION_PROTOCOL_DEFINITION ( 'draft international standard', 'automotive_design', 1998, #3407 ) ;
#6955 = DIRECTION ( 'NONE',  ( 0.000000000000000000, 0.000000000000000000, 1.000000000000000000 ) ) ;
#6956 = CARTESIAN_POINT ( 'NONE',  ( -1.900666315163639597, 43.27090656005016456, -136.0552959530036219 ) ) ;
#6957 = EDGE_CURVE ( 'NONE', #22660, #16248, #5979, .T. ) ;
#6958 = CARTESIAN_POINT ( 'NONE',  ( -13.50000000000000000, -43.00000000000000000, -136.0552959530000123 ) ) ;
#6959 = EDGE_LOOP ( 'NONE', ( #14711, #20420, #16785, #12576 ) ) ;
#6960 = EDGE_CURVE ( 'NONE', #14794, #23501, #1470, .T. ) ;
#6961 = CARTESIAN_POINT ( 'NONE',  ( -23.75346069390047887, 38.76012023700184983, -139.9914357966623015 ) ) ;
#6962 = VERTEX_POINT ( 'NONE', #17998 ) ;
#6963 =( NAMED_UNIT ( * ) SI_UNIT ( $, .STERADIAN. ) SOLID_ANGLE_UNIT ( ) );
#6964 = VERTEX_POINT ( 'NONE', #3355 ) ;
#6965 = LINE ( 'NONE', #18035, #9493 ) ;
#6966 = CARTESIAN_POINT ( 'NONE',  ( -28.85277900879999891, 34.87340808660000135, -141.1101275619999740 ) ) ;
#6967 = ORIENTED_EDGE ( 'NONE', *, *, #13158, .F. ) ;
#6968 = DIRECTION ( 'NONE',  ( 1.527666881879999979E-13, 8.171241461240000022E-13, 1.000000000000000000 ) ) ;
#6969 = VERTEX_POINT ( 'NONE', #6687 ) ;
#6970 = CARTESIAN_POINT ( 'NONE',  ( 22.89765167460447870, 39.50000000000002842, -136.0552959530517398 ) ) ;
#6971 = B_SPLINE_CURVE_WITH_KNOTS ( 'NONE', 5,
 ( #7261, #9491, #15095, #14873, #22014, #20345, #2266, #7826, #22131, #4040, #11507, #16764 ),
 .UNSPECIFIED., .F., .F.,
 ( 6, 3, 3, 6 ),
 ( 0.000000000000000000, 4.564346237179999655, 9.066392868600001265, 13.51003987140000007 ),
 .UNSPECIFIED. ) ;
#6972 = CARTESIAN_POINT ( 'NONE',  ( -19.74460998602464201, 33.84556549679342652, -142.4254691117371578 ) ) ;
#6973 = CARTESIAN_POINT ( 'NONE',  ( -12.22876056493469221, 38.35711075933631520, -147.2541758749702581 ) ) ;
#6974 = EDGE_CURVE ( 'NONE', #7890, #17493, #23096, .T. ) ;
#6975 = PRODUCT_DEFINITION_FORMATION_WITH_SPECIFIED_SOURCE ( 'ANY', '', #179, .NOT_KNOWN. ) ;
#6976 = CARTESIAN_POINT ( 'NONE',  ( 18.95053822279999878, -50.00000000000000000, -149.5552959529999839 ) ) ;
#6977 = VERTEX_POINT ( 'NONE', #8817 ) ;
#6978 = DIRECTION ( 'NONE',  ( 1.000000000000000000, 0.000000000000000000, -2.775557561562892298E-14 ) ) ;
#6979 = AXIS2_PLACEMENT_3D ( 'NONE', #8298, #9317, #1867 ) ;
#6980 = ORIENTED_EDGE ( 'NONE', *, *, #10262, .T. ) ;
#6981 = CARTESIAN_POINT ( 'NONE',  ( 9.876586606239635913, 36.40403110125505037, -141.6273462229582947 ) ) ;
#6982 = DIRECTION ( 'NONE',  ( 2.506794771760000178E-12, 5.921189464669999937E-17, -1.000000000000000000 ) ) ;
#6983 = DIRECTION ( 'NONE',  ( 1.000000000000000000, 0.000000000000000000, 2.516505522483685870E-12 ) ) ;
#6984 = ORIENTED_EDGE ( 'NONE', *, *, #19180, .T. ) ;
#6985 = EDGE_CURVE ( 'NONE', #1369, #21363, #3136, .T. ) ;
#6986 = DIRECTION ( 'NONE',  ( 2.255973186040000320E-12, 0.000000000000000000, 1.000000000000000000 ) ) ;
#6987 = ORIENTED_EDGE ( 'NONE', *, *, #18400, .F. ) ;
#6988 = FACE_OUTER_BOUND ( 'NONE', #13081, .T. ) ;
#6989 = ADVANCED_FACE ( 'NONE', ( #23115, #14425 ), #6806, .T. ) ;
#6990 = CARTESIAN_POINT ( 'NONE',  ( -31.00000000000000000, 1.000000000000000000, -150.0552959529999839 ) ) ;
#6991 = EDGE_LOOP ( 'NONE', ( #7990, #18897, #23423, #18722 ) ) ;
#6992 = CARTESIAN_POINT ( 'NONE',  ( 22.00000000000000000, -20.50000000000000000, -137.0552959530000123 ) ) ;
#6993 = ORIENTED_EDGE ( 'NONE', *, *, #4594, .T. ) ;
#6994 = VECTOR ( 'NONE', #517, 1000.000000000000000 ) ;
#6995 = CARTESIAN_POINT ( 'NONE',  ( -21.33871772395523791, 34.54066873271768401, -147.2646375961022045 ) ) ;
#6996 = CARTESIAN_POINT ( 'NONE',  ( -29.13601448249999848, 36.98639052360000079, -140.5419328609999923 ) ) ;
#6997 = VERTEX_POINT ( 'NONE', #12274 ) ;
#6998 = CARTESIAN_POINT ( 'NONE',  ( 0.000000000000000000, 0.000000000000000000, 0.000000000000000000 ) ) ;
#6999 = EDGE_LOOP ( 'NONE', ( #16415, #2791, #10914, #4335 ) ) ;
#7000 = CARTESIAN_POINT ( 'NONE',  ( -26.22336464713773196, 39.81244140399248721, -140.1811132391529497 ) ) ;
#7001 = LINE ( 'NONE', #12585, #23271 ) ;
#7002 = VERTEX_POINT ( 'NONE', #19548 ) ;
#7003 = DIRECTION ( 'NONE',  ( 1.000000000000000000, 0.000000000000000000, -2.257453483404485639E-12 ) ) ;
#7004 = DIRECTION ( 'NONE',  ( -1.000000000000000000, 0.000000000000000000, -1.457985068979999943E-12 ) ) ;
#7005 = VERTEX_POINT ( 'NONE', #3241 ) ;
#7006 = CARTESIAN_POINT ( 'NONE',  ( -13.64404366370000155, 33.71937897319999422, -142.3027892629999940 ) ) ;
#7007 = AXIS2_PLACEMENT_3D ( 'NONE', #21208, #22741, #5018 ) ;
#7008 = ORIENTED_EDGE ( 'NONE', *, *, #2068, .T. ) ;
#7009 = LINE ( 'NONE', #3324, #4445 ) ;
#7010 = CARTESIAN_POINT ( 'NONE',  ( 31.50000000000000000, -21.03620104879999886, -137.0552959530000123 ) ) ;
#7011 = CARTESIAN_POINT ( 'NONE',  ( -14.83278250960868050, 40.60058613835127517, -144.4189779529964142 ) ) ;
#7012 = CARTESIAN_POINT ( 'NONE',  ( 3.061723384069999998, -6.132747685670000060, -135.0552959530000123 ) ) ;
#7013 = VERTEX_POINT ( 'NONE', #10476 ) ;
#7014 = CARTESIAN_POINT ( 'NONE',  ( 1.544882029700253234, 14.84887268567989338, -136.0552959530035082 ) ) ;
#7015 = EDGE_CURVE ( 'NONE', #4660, #19550, #20898, .T. ) ;
#7016 = CARTESIAN_POINT ( 'NONE',  ( -26.17844700328911145, 36.98132551454334305, -140.6351982806022818 ) ) ;
#7017 = CARTESIAN_POINT ( 'NONE',  ( 4.499999999879999102, -3.500000000000000000, -136.0552959530000123 ) ) ;
#7018 = DIRECTION ( 'NONE',  ( 0.000000000000000000, -1.000000000000000000, 0.000000000000000000 ) ) ;
#7019 = CARTESIAN_POINT ( 'NONE',  ( -24.97797643630000053, 37.05442817780000553, -147.8575004449999994 ) ) ;
#7020 = FACE_OUTER_BOUND ( 'NONE', #20341, .T. ) ;
#7021 = ORIENTED_EDGE ( 'NONE', *, *, #22844, .T. ) ;
#7022 = DIRECTION ( 'NONE',  ( -1.000000000000000000, 0.000000000000000000, 2.257495777610000006E-12 ) ) ;
#7023 = CARTESIAN_POINT ( 'NONE',  ( 6.500000000140000012, 20.50000000000000000, -146.5552959529999839 ) ) ;
#7024 = LINE ( 'NONE', #14536, #9824 ) ;
#7025 = ADVANCED_FACE ( 'NONE', ( #11070 ), #18572, .F. ) ;
#7026 = VECTOR ( 'NONE', #3744, 1000.000000000000000 ) ;
#7027 = CARTESIAN_POINT ( 'NONE',  ( -6.464115716629577513, 37.99579816708060065, -148.7400127089275372 ) ) ;
#7028 = CARTESIAN_POINT ( 'NONE',  ( -21.35824191589999899, -32.00000000000000000, -146.2257682199999920 ) ) ;
#7029 = DIRECTION ( 'NONE',  ( 1.000000000000000000, 0.000000000000000000, 2.516505522483685870E-12 ) ) ;
#7030 = ORIENTED_EDGE ( 'NONE', *, *, #574, .T. ) ;
#7031 = CARTESIAN_POINT ( 'NONE',  ( 32.00000000000000000, 20.96379895120000114, -136.0552959530000123 ) ) ;
#7032 = PLANE ( 'NONE',  #20835 ) ;
#7033 = ORIENTED_EDGE ( 'NONE', *, *, #7758, .T. ) ;
#7034 = EDGE_CURVE ( 'NONE', #6268, #18451, #2171, .T. ) ;
#7035 = CARTESIAN_POINT ( 'NONE',  ( 21.39890631740000160, -21.26106171180000359, -145.5552959529999839 ) ) ;
#7036 = VERTEX_POINT ( 'NONE', #5607 ) ;
#7037 = CARTESIAN_POINT ( 'NONE',  ( -24.56431249151015805, 39.13927797951933485, -146.9768926602517354 ) ) ;
#7038 = CARTESIAN_POINT ( 'NONE',  ( -29.93285177491310378, 39.00107643762004273, -140.4906359816092447 ) ) ;
#7039 = CARTESIAN_POINT ( 'NONE',  ( 5.631397321050000571, -17.85059010000000157, -147.5552959529999839 ) ) ;
#7040 = CARTESIAN_POINT ( 'NONE',  ( 7.960302519239492725, 38.39964962483306010, -141.9838786040258469 ) ) ;
#7041 = VECTOR ( 'NONE', #970, 1000.000000000000000 ) ;
#7042 = ORIENTED_EDGE ( 'NONE', *, *, #16058, .F. ) ;
#7043 = DIRECTION ( 'NONE',  ( 0.000000000000000000, 1.000000000000000000, 0.000000000000000000 ) ) ;
#7044 = EDGE_CURVE ( 'NONE', #5708, #10881, #2296, .T. ) ;
#7045 = DIRECTION ( 'NONE',  ( 0.07970438983373200059, 0.9968185442904001770, -8.242295734823311485E-13 ) ) ;
#7046 = DIRECTION ( 'NONE',  ( -1.000000000000000000, 1.156482317317871331E-15, 2.257453483404484831E-12 ) ) ;
#7047 = DIRECTION ( 'NONE',  ( 1.000000000000000000, 0.000000000000000000, -8.955799065309598247E-12 ) ) ;
#7048 = ORIENTED_EDGE ( 'NONE', *, *, #9356, .F. ) ;
#7049 = CARTESIAN_POINT ( 'NONE',  ( 17.57628698946902901, 21.71923945895291652, -136.0552959530396890 ) ) ;
#7050 =( NAMED_UNIT ( * ) SI_UNIT ( $, .STERADIAN. ) SOLID_ANGLE_UNIT ( ) );
#7051 = APPLICATION_CONTEXT ( 'automotive_design' ) ;
#7052 = ADVANCED_FACE ( 'NONE', ( #16552 ), #7621, .T. ) ;
#7053 = VERTEX_POINT ( 'NONE', #4061 ) ;
#7054 = CARTESIAN_POINT ( 'NONE',  ( -7.500000000000000000, 22.50000000000000000, -150.0552959529999839 ) ) ;
#7055 = CARTESIAN_POINT ( 'NONE',  ( -21.35824191591069265, -4.000000000000000000, -141.9623572383524959 ) ) ;
#7056 = CARTESIAN_POINT ( 'NONE',  ( -4.881030538545268804, 24.01480899505181554, -136.0552959529889847 ) ) ;
#7057 = ADVANCED_FACE ( 'NONE', ( #15002 ), #152, .T. ) ;
#7058 = EDGE_LOOP ( 'NONE', ( #10727, #12467, #2139, #13469 ) ) ;
#7059 = CARTESIAN_POINT ( 'NONE',  ( -30.99999999989999822, 47.50000000000000000, -139.0552959529999839 ) ) ;
#7060 = DIRECTION ( 'NONE',  ( 0.000000000000000000, 0.000000000000000000, 1.000000000000000000 ) ) ;
#7061 = AXIS2_PLACEMENT_3D ( 'NONE', #15713, #12014, #19278 ) ;
#7062 = VECTOR ( 'NONE', #21723, 1000.000000000000000 ) ;
#7063 = EDGE_LOOP ( 'NONE', ( #2861, #6023, #3078, #12633 ) ) ;
#7064 = FACE_OUTER_BOUND ( 'NONE', #6139, .T. ) ;
#7065 = EDGE_CURVE ( 'NONE', #11626, #19736, #20365, .T. ) ;
#7066 = CARTESIAN_POINT ( 'NONE',  ( 17.50006728695150215, 22.10251055745073501, -150.0552959529999839 ) ) ;
#7067 = ADVANCED_FACE ( 'NONE', ( #19902, #7395 ), #9517, .T. ) ;
#7068 = CARTESIAN_POINT ( 'NONE',  ( -13.69054896997999826, -43.75739788393685359, -150.0552959529999839 ) ) ;
#7069 = CARTESIAN_POINT ( 'NONE',  ( 3.000000000000000000, -3.500000000000000000, -145.5552959529999839 ) ) ;
#7070 = EDGE_CURVE ( 'NONE', #22660, #8011, #1948, .T. ) ;
#7071 = DIRECTION ( 'NONE',  ( 1.000000000000000000, 2.602084704489999637E-17, -1.701177084830000066E-20 ) ) ;
#7072 = EDGE_CURVE ( 'NONE', #18341, #4286, #16790, .T. ) ;
#7073 = CARTESIAN_POINT ( 'NONE',  ( -26.39607007120000048, 36.95534867429999792, -140.3840478969999879 ) ) ;
#7074 = PRODUCT_CONTEXT ( 'NONE', #4627, 'mechanical' ) ;
#7075 = CYLINDRICAL_SURFACE ( 'NONE', #22297, 2.000000000000001776 ) ;
#7076 = CARTESIAN_POINT ( 'NONE',  ( -1.499999999959999331, 44.23820061220084199, -136.0552959530045314 ) ) ;
#7077 = FACE_OUTER_BOUND ( 'NONE', #4271, .T. ) ;
#7078 = ORIENTED_EDGE ( 'NONE', *, *, #9306, .T. ) ;
#7079 = CIRCLE ( 'NONE', #4042, 5.000000000000000000 ) ;
#7080 = AXIS2_PLACEMENT_3D ( 'NONE', #18373, #10857, #18139 ) ;
#7081 = UNCERTAINTY_MEASURE_WITH_UNIT (LENGTH_MEASURE( 1.000000000000000082E-05 ), #23244, 'distance_accuracy_value', 'NONE');
#7082 = ORIENTED_EDGE ( 'NONE', *, *, #8583, .F. ) ;
#7083 = SURFACE_STYLE_USAGE ( .BOTH. , #19697 ) ;
#7084 = ORIENTED_EDGE ( 'NONE', *, *, #15487, .T. ) ;
#7085 = CARTESIAN_POINT ( 'NONE',  ( -15.67014142446072178, 35.45905754578375024, -147.3461856841366000 ) ) ;
#7086 = CYLINDRICAL_SURFACE ( 'NONE', #12217, 6.000000000000002665 ) ;
#7087 = ORIENTED_EDGE ( 'NONE', *, *, #6903, .T. ) ;
#7088 = CARTESIAN_POINT ( 'NONE',  ( -15.00000000000000000, -43.00000000000000000, -145.5552959529999839 ) ) ;
#7089 = ORIENTED_EDGE ( 'NONE', *, *, #3711, .F. ) ;
#7090 = CARTESIAN_POINT ( 'NONE',  ( -6.477935707790000386, -19.20465386649999928, -147.5552959529999839 ) ) ;
#7091 = CARTESIAN_POINT ( 'NONE',  ( -20.54812748657687038, 36.93719815735425271, -140.4704715740689949 ) ) ;
#7092 = CARTESIAN_POINT ( 'NONE',  ( -11.92782157744108140, 37.65756807781640703, -147.5967280858595245 ) ) ;
#7093 = FACE_OUTER_BOUND ( 'NONE', #9335, .T. ) ;
#7094 = ORIENTED_EDGE ( 'NONE', *, *, #19127, .F. ) ;
#7095 = CARTESIAN_POINT ( 'NONE',  ( -6.083910486889999802, -15.16899799649999991, -144.5552959529999839 ) ) ;
#7096 = ORIENTED_EDGE ( 'NONE', *, *, #5237, .T. ) ;
#7097 = CARTESIAN_POINT ( 'NONE',  ( -9.157754307290000284, -15.75963164970000108, -147.5552959529999839 ) ) ;
#7098 = EDGE_CURVE ( 'NONE', #7777, #634, #1822, .T. ) ;
#7099 = AXIS2_PLACEMENT_3D ( 'NONE', #9196, #176, #1737 ) ;
#7100 = CARTESIAN_POINT ( 'NONE',  ( 4.500000000009999113, -5.000000000000000000, -136.0552959530000123 ) ) ;
#7101 = FACE_OUTER_BOUND ( 'NONE', #21443, .T. ) ;
#7102 = VERTEX_POINT ( 'NONE', #11182 ) ;
#7103 = LINE ( 'NONE', #10534, #3857 ) ;
#7104 = VERTEX_POINT ( 'NONE', #503 ) ;
#7105 = CARTESIAN_POINT ( 'NONE',  ( -18.85469010170000459, 37.03971195569999963, -148.4264296979999926 ) ) ;
#7106 = DIRECTION ( 'NONE',  ( 1.000000000000000000, 0.000000000000000000, 0.000000000000000000 ) ) ;
#7108 = EDGE_LOOP ( 'NONE', ( #4503, #13044 ) ) ;
#7107 = CIRCLE ( 'NONE', #14701, 7.000000000000000888 ) ;
#7109 = CARTESIAN_POINT ( 'NONE',  ( -11.53909816450000037, 41.50279269539999660, -144.7127947380000137 ) ) ;
#7110 = EDGE_LOOP ( 'NONE', ( #23352, #1144, #10089, #21539, #13397, #1941 ) ) ;
#7111 = LINE ( 'NONE', #12577, #19741 ) ;
#7112 = CIRCLE ( 'NONE', #7859, 2.500000000000000444 ) ;
#7113 = CARTESIAN_POINT ( 'NONE',  ( -35.07300000000000040, 14.00000000000000000, -144.0552959529999839 ) ) ;
#7114 = ORIENTED_EDGE ( 'NONE', *, *, #6593, .F. ) ;
#7115 = ORIENTED_EDGE ( 'NONE', *, *, #20640, .F. ) ;
#7116 = CARTESIAN_POINT ( 'NONE',  ( 19.13369214859999801, -50.50000000000000000, -136.0552959530000123 ) ) ;
#7117 = EDGE_CURVE ( 'NONE', #22329, #14876, #7736, .T. ) ;
#7118 = DIRECTION ( 'NONE',  ( 1.000000000000000000, 0.000000000000000000, -4.430318231639999944E-12 ) ) ;
#7119 = ORIENTED_EDGE ( 'NONE', *, *, #14942, .T. ) ;
#7120 = DIRECTION ( 'NONE',  ( 1.000000000000000000, 0.000000000000000000, -2.257453483404482811E-12 ) ) ;
#7121 = LINE ( 'NONE', #5345, #19386 ) ;
#7122 = EDGE_CURVE ( 'NONE', #10437, #15057, #7281, .T. ) ;
#7123 = CARTESIAN_POINT ( 'NONE',  ( -6.657076963140000636, -20.13603737529999904, -144.5552959529999839 ) ) ;
#7124 = VERTEX_POINT ( 'NONE', #12744 ) ;
#7125 = CARTESIAN_POINT ( 'NONE',  ( -16.63107678139999734, 35.60580843630000203, -140.6802342589999739 ) ) ;
#7126 = VECTOR ( 'NONE', #4185, 1000.000000000000000 ) ;
#7127 = VECTOR ( 'NONE', #19277, 1000.000000000000000 ) ;
#7128 = ORIENTED_EDGE ( 'NONE', *, *, #959, .T. ) ;
#7129 = CARTESIAN_POINT ( 'NONE',  ( -15.50000000000000000, 0.000000000000000000, -150.0552959529999839 ) ) ;
#7130 = LINE ( 'NONE', #8782, #579 ) ;
#7131 = CARTESIAN_POINT ( 'NONE',  ( 10.93320006080000084, -15.50000000000000000, -150.0552959529999839 ) ) ;
#7132 = CARTESIAN_POINT ( 'NONE',  ( -28.72360428835138535, 40.14058537508078928, -141.1268109065168801 ) ) ;
#7133 = VERTEX_POINT ( 'NONE', #20017 ) ;
#7134 = FACE_OUTER_BOUND ( 'NONE', #23306, .T. ) ;
#7135 = DIRECTION ( 'NONE',  ( 2.257144641399999941E-12, 0.000000000000000000, -1.000000000000000000 ) ) ;
#7136 = DIRECTION ( 'NONE',  ( 4.430318231639999944E-12, -6.100259101500000139E-13, 1.000000000000000000 ) ) ;
#7137 = DIRECTION ( 'NONE',  ( 1.000000000000000000, 0.000000000000000000, 0.000000000000000000 ) ) ;
#7138 = LINE ( 'NONE', #19883, #8023 ) ;
#7139 = DIRECTION ( 'NONE',  ( 0.6459422414661276646, -0.7633862853691535388, 2.257453483404482811E-12 ) ) ;
#7140 = VERTEX_POINT ( 'NONE', #2864 ) ;
#7141 = CARTESIAN_POINT ( 'NONE',  ( 0.5000000001590284571, 24.10555127549999810, -139.5552959530157864 ) ) ;
#7142 = VECTOR ( 'NONE', #8696, 1000.000000000000114 ) ;
#7143 = DIRECTION ( 'NONE',  ( 0.000000000000000000, 0.000000000000000000, 1.000000000000000000 ) ) ;
#7144 = CARTESIAN_POINT ( 'NONE',  ( -13.60030749279999895, 34.19157895370000233, -140.3499153360000093 ) ) ;
#7145 = CARTESIAN_POINT ( 'NONE',  ( -6.244164552826013015, 39.88079648725181414, -147.9541347234863622 ) ) ;
#7146 = CARTESIAN_POINT ( 'NONE',  ( -14.60737817346108258, -44.46095901500248004, -136.0552959530008934 ) ) ;
#7147 = ORIENTED_EDGE ( 'NONE', *, *, #1878, .F. ) ;
#7148 = ADVANCED_FACE ( 'NONE', ( #1086 ), #19158, .F. ) ;
#7149 = CARTESIAN_POINT ( 'NONE',  ( -18.35824191589999899, -1.500000000000000000, -148.1907682189999775 ) ) ;
#7150 = CARTESIAN_POINT ( 'NONE',  ( -7.149448239889999890, -25.45628515800000002, -146.5552959529999839 ) ) ;
#7151 = ADVANCED_FACE ( 'NONE', ( #13208 ), #17015, .T. ) ;
#7152 = ORIENTED_EDGE ( 'NONE', *, *, #2280, .F. ) ;
#7153 = PLANE ( 'NONE',  #750 ) ;
#7154 = ORIENTED_EDGE ( 'NONE', *, *, #12164, .F. ) ;
#7155 = DIRECTION ( 'NONE',  ( -1.000000000000000000, 5.094701932209999624E-24, 2.257144641399999941E-12 ) ) ;
#7156 = AXIS2_PLACEMENT_3D ( 'NONE', #20189, #3885, #11118 ) ;
#7157 = CARTESIAN_POINT ( 'NONE',  ( -29.62827070404598118, 36.92763176543375891, -139.7399851633028618 ) ) ;
#7158 = CIRCLE ( 'NONE', #20096, 2.000000000000000000 ) ;
#7159 = DIRECTION ( 'NONE',  ( 2.257749542879999954E-12, 0.000000000000000000, 1.000000000000000000 ) ) ;
#7160 = CARTESIAN_POINT ( 'NONE',  ( 7.123413393902458424, 37.59596889877142445, -141.6273462229617621 ) ) ;
#7161 = ORIENTED_EDGE ( 'NONE', *, *, #22668, .T. ) ;
#7162 = CARTESIAN_POINT ( 'NONE',  ( -10.96486579892240520, 34.29678926733738820, -140.1220017724852482 ) ) ;
#7163 = CARTESIAN_POINT ( 'NONE',  ( -19.13109106545264737, 32.92487917598572267, -146.6426253244906945 ) ) ;
#7164 = CARTESIAN_POINT ( 'NONE',  ( -9.870393330421920908, 37.85345449832967546, -147.8311166192347912 ) ) ;
#7165 = DIRECTION ( 'NONE',  ( -1.000000000000000000, 0.000000000000000000, 2.275957200481568888E-12 ) ) ;
#7166 = ORIENTED_EDGE ( 'NONE', *, *, #5932, .F. ) ;
#7167 = CARTESIAN_POINT ( 'NONE',  ( 18.98502865247582960, 25.11890206003844384, -136.0552959530428723 ) ) ;
#7168 = EDGE_CURVE ( 'NONE', #361, #1717, #966, .T. ) ;
#7169 = ORIENTED_EDGE ( 'NONE', *, *, #9488, .T. ) ;
#7170 = DIRECTION ( 'NONE',  ( -2.891205793294675861E-15, -1.000000000000000000, 0.000000000000000000 ) ) ;
#7171 = CARTESIAN_POINT ( 'NONE',  ( -2.499999999959999997, 34.00000000000000000, -153.0552959529999839 ) ) ;
#7172 = PLANE ( 'NONE',  #20680 ) ;
#7173 = AXIS2_PLACEMENT_3D ( 'NONE', #18657, #11150, #7698 ) ;
#7174 = ORIENTED_EDGE ( 'NONE', *, *, #12402, .F. ) ;
#7175 = CARTESIAN_POINT ( 'NONE',  ( -5.096343650290934058, 36.99112588043591643, -140.7242647647981073 ) ) ;
#7176 = DIRECTION ( 'NONE',  ( 1.000000000000000000, 0.000000000000000000, -2.257171095940000041E-12 ) ) ;
#7177 = CIRCLE ( 'NONE', #1489, 8.176568160360000448 ) ;
#7178 = EDGE_CURVE ( 'NONE', #19530, #11089, #12058, .T. ) ;
#7179 = ORIENTED_EDGE ( 'NONE', *, *, #23218, .T. ) ;
#7180 = PLANE ( 'NONE',  #4581 ) ;
#7181 = VECTOR ( 'NONE', #4287, 1000.000000000000000 ) ;
#7182 = CIRCLE ( 'NONE', #20863, 8.176568160360000448 ) ;
#7183 = CARTESIAN_POINT ( 'NONE',  ( -3.500000048370000005, 39.19395640469999620, -145.2538597999999865 ) ) ;
#7184 = DIRECTION ( 'NONE',  ( 1.000000000000000000, -5.094701941669999797E-24, -2.257144641399999941E-12 ) ) ;
#7185 = CARTESIAN_POINT ( 'NONE',  ( 8.496192186321144035, -45.75965300677037106, -136.0552959530191970 ) ) ;
#7186 = FACE_OUTER_BOUND ( 'NONE', #21980, .T. ) ;
#7187 = ADVANCED_FACE ( 'NONE', ( #6305 ), #19041, .F. ) ;
#7188 = PLANE ( 'NONE',  #3700 ) ;
#7189 = ITEM_DEFINED_TRANSFORMATION ( 'NONE', 'NONE', #16842,  #5025 ) ;
#7190 = CARTESIAN_POINT ( 'NONE',  ( -2.499999999959999997, 34.00000000000000000, -151.5552959529999839 ) ) ;
#7191 = DIRECTION ( 'NONE',  ( -5.094701932209999624E-24, -1.000000000000000000, 1.149947916579999802E-35 ) ) ;
#7192 = AXIS2_PLACEMENT_3D ( 'NONE', #13468, #15380, #11443 ) ;
#7193 = CARTESIAN_POINT ( 'NONE',  ( 2.508811538190000245, -14.35090895149999923, -145.5552959529999839 ) ) ;
#7194 = VECTOR ( 'NONE', #2930, 1000.000000000000000 ) ;
#7195 = EDGE_LOOP ( 'NONE', ( #2436, #19501, #10737 ) ) ;
#7196 =( BOUNDED_SURFACE ( )  B_SPLINE_SURFACE ( 5, 5, ( 
 ( #16479, #18151, #12902, #20183, #5425, #22077 ),
 ( #1865, #12546, #3984, #3873, #16135, #16588 ),
 ( #18036, #1747, #7541, #3638, #14819, #13023 ),
 ( #21735, #12669, #10873, #7322, #20524, #15394 ),
 ( #9428, #9779, #4336, #22540, #16709, #650 ),
 ( #13369, #5876, #2448, #4449, #17055, #9666 ),
 ( #6348, #17179, #22190, #2209, #22653, #543 ),
 ( #11808, #11333, #9557, #2555, #11684, #6234 ),
 ( #18963, #13248, #13482, #4221, #16941, #13602 ),
 ( #7660, #18618, #778, #7883, #2677, #422 ),
 ( #8004, #6115, #20875, #15286, #11457, #18738 ),
 ( #4097, #8121, #20643, #15161, #22423, #11569 ) ),
 .UNSPECIFIED., .F., .F., .F. ) 
 B_SPLINE_SURFACE_WITH_KNOTS ( ( 6, 3, 3, 6 ),
 ( 6, 6 ),
 ( 0.000000000000000000, 4.066159495680000013, 8.252146144990000209, 12.56898909050000057 ),
 ( 1.570796326630355066, 3.141592653590000062 ),
 .UNSPECIFIED. ) 
 GEOMETRIC_REPRESENTATION_ITEM ( )  RATIONAL_B_SPLINE_SURFACE ( (
 ( 0.2500000000000000000, 0.2499999999790369909, 0.2999999999685555307, 0.3999999999580740040, 0.5999999999580739596, 1.000000000000000000),
 ( 0.2500000000000000000, 0.2499999999790369909, 0.2999999999685555307, 0.3999999999580740040, 0.5999999999580739596, 1.000000000000000000),
 ( 0.2500000000000000000, 0.2499999999790369909, 0.2999999999685555307, 0.3999999999580740040, 0.5999999999580739596, 1.000000000000000000),
 ( 0.2500000000000000000, 0.2499999999790369909, 0.2999999999685555307, 0.3999999999580740040, 0.5999999999580739596, 1.000000000000000000),
 ( 0.2500000000000000000, 0.2499999999790369909, 0.2999999999685555307, 0.3999999999580740040, 0.5999999999580739596, 1.000000000000000000),
 ( 0.2500000000000000000, 0.2499999999790369909, 0.2999999999685555307, 0.3999999999580740040, 0.5999999999580739596, 1.000000000000000000),
 ( 0.2500000000000000000, 0.2499999999790369909, 0.2999999999685555307, 0.3999999999580740040, 0.5999999999580739596, 1.000000000000000000),
 ( 0.2500000000000000000, 0.2499999999790369909, 0.2999999999685555307, 0.3999999999580740040, 0.5999999999580739596, 1.000000000000000000),
 ( 0.2500000000000000000, 0.2499999999790369909, 0.2999999999685555307, 0.3999999999580740040, 0.5999999999580739596, 1.000000000000000000),
 ( 0.2500000000000000000, 0.2499999999790369909, 0.2999999999685555307, 0.3999999999580740040, 0.5999999999580739596, 1.000000000000000000),
 ( 0.2500000000000000000, 0.2499999999790369909, 0.2999999999685555307, 0.3999999999580740040, 0.5999999999580739596, 1.000000000000000000),
 ( 0.2500000000000000000, 0.2499999999790369909, 0.2999999999685555307, 0.3999999999580740040, 0.5999999999580739596, 1.000000000000000000) ) ) 
 REPRESENTATION_ITEM ( '' )  SURFACE ( )  );
#7197 = VERTEX_POINT ( 'NONE', #8195 ) ;
#7198 = PRESENTATION_STYLE_ASSIGNMENT (( #12666 ) ) ;
#7199 = ADVANCED_FACE ( 'NONE', ( #20957 ), #11529, .F. ) ;
#7200 = VECTOR ( 'NONE', #21154, 1000.000000000000000 ) ;
#7201 = EDGE_CURVE ( 'NONE', #20840, #10047, #7847, .T. ) ;
#7202 = ORIENTED_EDGE ( 'NONE', *, *, #12190, .F. ) ;
#7203 = CARTESIAN_POINT ( 'NONE',  ( 18.95053822279999878, -50.00000000000000000, -150.0552959529999839 ) ) ;
#7204 = CARTESIAN_POINT ( 'NONE',  ( -2.499999999920000437, 34.00000000000000000, -135.0552959530000123 ) ) ;
#7205 = VERTEX_POINT ( 'NONE', #20830 ) ;
#7206 = LINE ( 'NONE', #19827, #2072 ) ;
#7207 = EDGE_CURVE ( 'NONE', #10920, #22797, #22724, .T. ) ;
#7208 = ORIENTED_EDGE ( 'NONE', *, *, #9532, .T. ) ;
#7209 = CARTESIAN_POINT ( 'NONE',  ( -4.576286989421689988, 23.28076054106537995, -150.0552959529999839 ) ) ;
#7210 = EDGE_CURVE ( 'NONE', #320, #19030, #13568, .T. ) ;
#7211 = CARTESIAN_POINT ( 'NONE',  ( -4.160432423080000497, -28.71743394529999804, -143.5552959529999839 ) ) ;
#7212 = CARTESIAN_POINT ( 'NONE',  ( -11.76172848620000089, 40.95326072219999958, -146.5101368410000191 ) ) ;
#7213 = DIRECTION ( 'NONE',  ( 1.000000000000000000, 0.000000000000000000, 0.000000000000000000 ) ) ;
#7214 = ORIENTED_EDGE ( 'NONE', *, *, #7611, .T. ) ;
#7215 = DIRECTION ( 'NONE',  ( 1.000000000000000000, 0.000000000000000000, -2.259303855112193156E-12 ) ) ;
#7216 = VECTOR ( 'NONE', #12564, 1000.000000000000227 ) ;
#7217 = ORIENTED_EDGE ( 'NONE', *, *, #1689, .T. ) ;
#7218 = CARTESIAN_POINT ( 'NONE',  ( 9.501873066115209099, 35.88348715183582982, -141.8183173552265828 ) ) ;
#7219 = AXIS2_PLACEMENT_3D ( 'NONE', #19453, #4575, #8487 ) ;
#7220 = VECTOR ( 'NONE', #9058, 1000.000000000000114 ) ;
#7221 = CARTESIAN_POINT ( 'NONE',  ( -15.50000000000000000, 47.50000000000000000, -136.5552959530000123 ) ) ;
#7222 = VECTOR ( 'NONE', #9716, 999.9999999999998863 ) ;
#7223 = AXIS2_PLACEMENT_3D ( 'NONE', #17717, #14616, #10788 ) ;
#7224 = FACE_OUTER_BOUND ( 'NONE', #22650, .T. ) ;
#7225 = VERTEX_POINT ( 'NONE', #17258 ) ;
#7226 = CARTESIAN_POINT ( 'NONE',  ( -32.50000000000000000, 1.000000000000000000, -150.5552959529999839 ) ) ;
#7227 = EDGE_LOOP ( 'NONE', ( #2090, #6193, #13763, #10007 ) ) ;
#7228 = PLANE ( 'NONE',  #1469 ) ;
#7229 = DIRECTION ( 'NONE',  ( 0.9944529286486341046, -0.1051825684329612265, -4.469111776238355154E-12 ) ) ;
#7230 = VERTEX_POINT ( 'NONE', #20483 ) ;
#7231 = LINE ( 'NONE', #19730, #15288 ) ;
#7232 = EDGE_CURVE ( 'NONE', #963, #4709, #11890, .T. ) ;
#7233 = VERTEX_POINT ( 'NONE', #11418 ) ;
#7234 = CARTESIAN_POINT ( 'NONE',  ( -15.59320802965877917, 39.76776338515035292, -147.7580614746654817 ) ) ;
#7235 = EDGE_CURVE ( 'NONE', #1424, #19480, #22503, .T. ) ;
#7236 = DIRECTION ( 'NONE',  ( 0.000000000000000000, -1.000000000000000000, 0.000000000000000000 ) ) ;
#7237 = VERTEX_POINT ( 'NONE', #2411 ) ;
#7238 = DIRECTION ( 'NONE',  ( 1.000000000000000000, 0.000000000000000000, 0.000000000000000000 ) ) ;
#7239 = AXIS2_PLACEMENT_3D ( 'NONE', #21080, #17376, #3220 ) ;
#7240 = ORIENTED_EDGE ( 'NONE', *, *, #13612, .T. ) ;
#7241 = CARTESIAN_POINT ( 'NONE',  ( -26.43221227920010463, 37.92234065499331308, -139.4358666115665812 ) ) ;
#7242 = CARTESIAN_POINT ( 'NONE',  ( -10.65913935279999869, 37.04331329920000115, -139.7140392919999954 ) ) ;
#7243 = EDGE_LOOP ( 'NONE', ( #22210, #18270, #15191, #21331 ) ) ;
#7244 = CARTESIAN_POINT ( 'NONE',  ( 25.50000000000000000, 19.50000000000000000, -136.0552959530000123 ) ) ;
#7245 = DIRECTION ( 'NONE',  ( 1.000000000000000000, 0.000000000000000000, 2.273736754430000208E-12 ) ) ;
#7246 = CARTESIAN_POINT ( 'NONE',  ( 17.66940543669999997, -18.68690163239999791, -144.5552959529999839 ) ) ;
#7247 = VERTEX_POINT ( 'NONE', #15117 ) ;
#7248 = CARTESIAN_POINT ( 'NONE',  ( -14.47770030809999930, -18.00000000000000000, -150.0552959529999839 ) ) ;
#7249 = CARTESIAN_POINT ( 'NONE',  ( -28.75749843875100709, 32.81834225557554419, -141.6071124201210694 ) ) ;
#7250 = VERTEX_POINT ( 'NONE', #20711 ) ;
#7251 = AXIS2_PLACEMENT_3D ( 'NONE', #8222, #1111, #10121 ) ;
#7252 = CARTESIAN_POINT ( 'NONE',  ( 8.500000000050000892, 37.00000000000000000, -146.5552959529999839 ) ) ;
#7253 = CARTESIAN_POINT ( 'NONE',  ( -20.62738678477109744, -4.195399377771871663, -146.3157682190057187 ) ) ;
#7254 = CARTESIAN_POINT ( 'NONE',  ( -16.64819173719487111, 39.54152330607143995, -140.6182326551606252 ) ) ;
#7255 = DIRECTION ( 'NONE',  ( 8.955190032050000935E-12, -9.104778821549999739E-13, 1.000000000000000000 ) ) ;
#7256 = ORIENTED_EDGE ( 'NONE', *, *, #9804, .F. ) ;
#7257 = DIRECTION ( 'NONE',  ( -0.000000000000000000, 1.000000000000000000, 0.000000000000000000 ) ) ;
#7258 = DIRECTION ( 'NONE',  ( 0.000000000000000000, -1.000000000000000000, -2.273736754430000208E-12 ) ) ;
#7259 = CARTESIAN_POINT ( 'NONE',  ( 6.000000000010000001, -3.500000000000000000, -136.5552959530000123 ) ) ;
#7260 = FACE_OUTER_BOUND ( 'NONE', #13525, .T. ) ;
#7261 = CARTESIAN_POINT ( 'NONE',  ( -27.77832206610000298, 37.03059619289999915, -147.6270870419999710 ) ) ;
#7262 = ADVANCED_FACE ( 'NONE', ( #17139 ), #22382, .F. ) ;
#7263 = FACE_OUTER_BOUND ( 'NONE', #13171, .T. ) ;
#7264 = ORIENTED_EDGE ( 'NONE', *, *, #3283, .F. ) ;
#7265 = CARTESIAN_POINT ( 'NONE',  ( -34.50000000000000000, 67.50000000000000000, -144.0552959529999839 ) ) ;
#7266 = DIRECTION ( 'NONE',  ( -1.000000000000000000, 5.094701932209999624E-24, 2.257144641399999941E-12 ) ) ;
#7267 = PLANE ( 'NONE',  #9447 ) ;
#7268 = CARTESIAN_POINT ( 'NONE',  ( -6.498948513254279469, 40.81543344996319433, -146.1568765785165738 ) ) ;
#7269 = VECTOR ( 'NONE', #9449, 1000.000000000000000 ) ;
#7270 = CARTESIAN_POINT ( 'NONE',  ( 2.499999999879999990, -4.000000000000000000, -135.0552959530000123 ) ) ;
#7271 = CLOSED_SHELL ( 'NONE', ( #394, #22310, #6502, #13035, #11291, #2332 ) ) ;
#7272 = AXIS2_PLACEMENT_3D ( 'NONE', #5070, #12313, #3281 ) ;
#7273 = ORIENTED_EDGE ( 'NONE', *, *, #22784, .F. ) ;
#7274 = CARTESIAN_POINT ( 'NONE',  ( -9.812199629320000227, -24.40642616239999896, -147.0552959529999839 ) ) ;
#7275 = LINE ( 'NONE', #14541, #9412 ) ;
#7276 = VERTEX_POINT ( 'NONE', #20601 ) ;
#7277 = FACE_OUTER_BOUND ( 'NONE', #21552, .T. ) ;
#7278 = ORIENTED_EDGE ( 'NONE', *, *, #13860, .T. ) ;
#7279 = LINE ( 'NONE', #5029, #15550 ) ;
#7280 = LINE ( 'NONE', #11069, #21136 ) ;
#7281 = LINE ( 'NONE', #14550, #18910 ) ;
#7282 = CARTESIAN_POINT ( 'NONE',  ( 7.156080887020574544, 36.33197188641598530, -141.6458064976851290 ) ) ;
#7283 = ORIENTED_EDGE ( 'NONE', *, *, #15099, .T. ) ;
#7284 = CARTESIAN_POINT ( 'NONE',  ( -32.00000000000000000, 1.000000000000000000, -149.5552959529999839 ) ) ;
#7285 = AXIS2_PLACEMENT_3D ( 'NONE', #8020, #16960, #18635 ) ;
#7286 = CLOSED_SHELL ( 'NONE', ( #12650, #210, #13498, #22757, #10675, #13149, #19430, #3575, #3830, #17172, #18109, #15420, #4460, #10265, #14194, #23208, #8585, #20543, #1467, #18250, #19870, #8935, #5106, #22782, #5441, #4583, #21049, #20400 ) ) ;
#7287 = CARTESIAN_POINT ( 'NONE',  ( -18.66256475003282489, 32.87452234919609850, -143.7440942753966056 ) ) ;
#7288 = AXIS2_PLACEMENT_3D ( 'NONE', #9502, #12967, #6184 ) ;
#7289 = DIRECTION ( 'NONE',  ( -0.9847555042252370550, 0.1739442350240419932, 7.083477032991710236E-15 ) ) ;
#7290 = CARTESIAN_POINT ( 'NONE',  ( 3.775218130429260022, -33.25714246578316136, -136.0552959530085673 ) ) ;
#7291 = ADVANCED_FACE ( 'NONE', ( #4300 ), #17835, .F. ) ;
#7292 = ORIENTED_EDGE ( 'NONE', *, *, #1006, .T. ) ;
#7293 = ADVANCED_FACE ( 'NONE', ( #20104, #1792, #21897 ), #7370, .F. ) ;
#7294 = FACE_OUTER_BOUND ( 'NONE', #19218, .T. ) ;
#7295 = ORIENTED_EDGE ( 'NONE', *, *, #3963, .T. ) ;
#7296 = CYLINDRICAL_SURFACE ( 'NONE', #15274, 2.999999999999999112 ) ;
#7297 = CARTESIAN_POINT ( 'NONE',  ( -5.659867863649999720, 38.70771930269999928, -140.0293976189999796 ) ) ;
#7298 = DIRECTION ( 'NONE',  ( 1.000000000000000000, 0.000000000000000000, 0.000000000000000000 ) ) ;
#7299 = ORIENTED_EDGE ( 'NONE', *, *, #8346, .T. ) ;
#7300 = FACE_OUTER_BOUND ( 'NONE', #14242, .T. ) ;
#7301 = CARTESIAN_POINT ( 'NONE',  ( -4.499999999919999105, 40.00000000000000000, -135.0552959530000123 ) ) ;
#7302 = AXIS2_PLACEMENT_3D ( 'NONE', #13075, #20576, #5704 ) ;
#7303 = CIRCLE ( 'NONE', #10698, 3.000000000000000000 ) ;
#7304 = ORIENTED_EDGE ( 'NONE', *, *, #14180, .F. ) ;
#7305 = AXIS2_PLACEMENT_3D ( 'NONE', #720, #18795, #18907 ) ;
#7306 = CARTESIAN_POINT ( 'NONE',  ( -18.18930989820000121, 36.96028804430000037, -147.6841622079999752 ) ) ;
#7307 = DIRECTION ( 'NONE',  ( 8.955190032050000935E-12, -9.104778821549999739E-13, 1.000000000000000000 ) ) ;
#7308 = CARTESIAN_POINT ( 'NONE',  ( -6.165211177139999776, -15.11551140080000089, -143.5552959529999839 ) ) ;
#7309 = CARTESIAN_POINT ( 'NONE',  ( -24.99548980002266774, 37.05651868163121065, -148.5304149360441386 ) ) ;
#7310 = DIRECTION ( 'NONE',  ( 0.000000000000000000, -3.386641135243274558E-17, -1.000000000000000000 ) ) ;
#7311 = CARTESIAN_POINT ( 'NONE',  ( 15.50000000000000000, 33.50000000000000000, -150.0552959529999839 ) ) ;
#7312 = CARTESIAN_POINT ( 'NONE',  ( 31.50000000000000000, 0.000000000000000000, -150.0552959529999839 ) ) ;
#7313 = DIRECTION ( 'NONE',  ( -0.9938526945756316344, 0.1107105301439589573, 6.178155812097707047E-14 ) ) ;
#7314 = DIRECTION ( 'NONE',  ( -1.000000000000000000, 0.000000000000000000, 2.257144641399999941E-12 ) ) ;
#7315 = ORIENTED_EDGE ( 'NONE', *, *, #11192, .F. ) ;
#7316 = ADVANCED_FACE ( 'NONE', ( #18430 ), #5810, .F. ) ;
#7317 = UNCERTAINTY_MEASURE_WITH_UNIT (LENGTH_MEASURE( 1.000000000000000082E-05 ), #15284, 'distance_accuracy_value', 'NONE');
#7318 = AXIS2_PLACEMENT_3D ( 'NONE', #1316, #11994, #2971 ) ;
#7319 = ORIENTED_EDGE ( 'NONE', *, *, #23058, .T. ) ;
#7320 = VERTEX_POINT ( 'NONE', #18201 ) ;
#7321 = CARTESIAN_POINT ( 'NONE',  ( 31.00000000000000000, -39.80430157320000006, -150.0552959529999839 ) ) ;
#7322 = CARTESIAN_POINT ( 'NONE',  ( -13.24550845540447597, 34.38214360666451341, -147.9047044067351635 ) ) ;
#7323 = ORIENTED_EDGE ( 'NONE', *, *, #14180, .T. ) ;
#7324 = CARTESIAN_POINT ( 'NONE',  ( -34.50000000000000000, -18.00000000000000000, -151.0552959529999839 ) ) ;
#7325 = ORIENTED_EDGE ( 'NONE', *, *, #21302, .T. ) ;
#7326 = CARTESIAN_POINT ( 'NONE',  ( -3.499999999969999998, 44.50000000000000000, -137.0552959530000123 ) ) ;
#7327 = ADVANCED_FACE ( 'NONE', ( #5579, #5694 ), #18539, .F. ) ;
#7328 = CARTESIAN_POINT ( 'NONE',  ( -18.75480078877485823, 35.03674905134475637, -146.9103430178364533 ) ) ;
#7329 = DIRECTION ( 'NONE',  ( -0.09606172499277214338, -0.9953753789357123738, 8.234154099303244678E-13 ) ) ;
#7330 = ORIENTED_EDGE ( 'NONE', *, *, #22193, .T. ) ;
#7331 = LINE ( 'NONE', #14354, #15609 ) ;
#7332 = ORIENTED_EDGE ( 'NONE', *, *, #1107, .F. ) ;
#7333 = CARTESIAN_POINT ( 'NONE',  ( 9.317029960348264694, 35.74200835522769637, -141.8948580844120784 ) ) ;
#7334 =( GEOMETRIC_REPRESENTATION_CONTEXT ( 3 ) GLOBAL_UNCERTAINTY_ASSIGNED_CONTEXT ( ( #13755 ) ) GLOBAL_UNIT_ASSIGNED_CONTEXT ( ( #17237, #8534, #2737 ) ) REPRESENTATION_CONTEXT ( 'NONE', 'WORKASPACE' ) );
#7335 = ADVANCED_FACE ( 'NONE', ( #5355 ), #23325, .F. ) ;
#7336 = DIRECTION ( 'NONE',  ( -1.000000000000000000, 0.000000000000000000, 0.000000000000000000 ) ) ;
#7337 = DIRECTION ( 'NONE',  ( -2.839308199620000013E-14, -3.568879590630000244E-13, -1.000000000000000000 ) ) ;
#7338 = ORIENTED_EDGE ( 'NONE', *, *, #9640, .T. ) ;
#7339 =( BOUNDED_SURFACE ( )  B_SPLINE_SURFACE ( 5, 5, ( 
 ( #17793, #8611, #10636, #6846, #14110, #1514 ),
 ( #12668, #8736, #16010, #23275, #8855, #23388 ),
 ( #7085, #14340, #12545, #8969, #19936, #3637 ),
 ( #13569, #20842, #17150, #15131, #18275, #11778 ),
 ( #13343, #12783, #19056, #20054, #17027, #20494 ),
 ( #16913, #9992, #3752, #22514, #870, #15368 ),
 ( #979, #4311, #746, #22625, #6316, #625 ),
 ( #7747, #185, #2767, #17270, #5533, #14583 ),
 ( #15013, #21851, #10996, #22274, #5966, #13219 ),
 ( #16478, #11541, #1985, #20616, #9208, #4194 ),
 ( #4537, #8096, #22393, #11431, #18714, #2422 ),
 ( #7858, #6091, #9639, #18817, #7977, #2529 ) ),
 .UNSPECIFIED., .F., .F., .F. ) 
 B_SPLINE_SURFACE_WITH_KNOTS ( ( 6, 3, 3, 6 ),
 ( 6, 6 ),
 ( 0.000000000000000000, 4.358589029760000066, 8.533830367689999363, 12.54112731390000057 ),
 ( 1.570796326654110064, 3.141592653590000062 ),
 .UNSPECIFIED. ) 
 GEOMETRIC_REPRESENTATION_ITEM ( )  RATIONAL_B_SPLINE_SURFACE ( (
 ( 0.2500000000000000000, 0.2499999999820609886, 0.2999999999730915134, 0.3999999999641219994, 0.5999999999641220105, 1.000000000000000000),
 ( 0.2500000000000000000, 0.2499999999820609886, 0.2999999999730915134, 0.3999999999641219994, 0.5999999999641220105, 1.000000000000000000),
 ( 0.2500000000000000000, 0.2499999999820609886, 0.2999999999730915134, 0.3999999999641219994, 0.5999999999641220105, 1.000000000000000000),
 ( 0.2500000000000000000, 0.2499999999820609886, 0.2999999999730915134, 0.3999999999641219994, 0.5999999999641220105, 1.000000000000000000),
 ( 0.2500000000000000000, 0.2499999999820609886, 0.2999999999730915134, 0.3999999999641219994, 0.5999999999641220105, 1.000000000000000000),
 ( 0.2500000000000000000, 0.2499999999820609886, 0.2999999999730915134, 0.3999999999641219994, 0.5999999999641220105, 1.000000000000000000),
 ( 0.2500000000000000000, 0.2499999999820609886, 0.2999999999730915134, 0.3999999999641219994, 0.5999999999641220105, 1.000000000000000000),
 ( 0.2500000000000000000, 0.2499999999820609886, 0.2999999999730915134, 0.3999999999641219994, 0.5999999999641220105, 1.000000000000000000),
 ( 0.2500000000000000000, 0.2499999999820609886, 0.2999999999730915134, 0.3999999999641219994, 0.5999999999641220105, 1.000000000000000000),
 ( 0.2500000000000000000, 0.2499999999820609886, 0.2999999999730915134, 0.3999999999641219994, 0.5999999999641220105, 1.000000000000000000),
 ( 0.2500000000000000000, 0.2499999999820609886, 0.2999999999730915134, 0.3999999999641219994, 0.5999999999641220105, 1.000000000000000000),
 ( 0.2500000000000000000, 0.2499999999820609886, 0.2999999999730915134, 0.3999999999641219994, 0.5999999999641220105, 1.000000000000000000) ) ) 
 REPRESENTATION_ITEM ( '' )  SURFACE ( )  );
#7340 = EDGE_CURVE ( 'NONE', #8156, #16928, #6274, .T. ) ;
#7341 = CARTESIAN_POINT ( 'NONE',  ( 8.500000000050000892, 37.00000000000000000, -146.5552959529999839 ) ) ;
#7342 = ORIENTED_EDGE ( 'NONE', *, *, #21957, .F. ) ;
#7343 = CARTESIAN_POINT ( 'NONE',  ( 4.750000000000000888, -47.26539404904927721, -150.0552959529999839 ) ) ;
#7344 = DIRECTION ( 'NONE',  ( 1.000000000000000000, 0.000000000000000000, 0.000000000000000000 ) ) ;
#7345 = ORIENTED_EDGE ( 'NONE', *, *, #23519, .F. ) ;
#7346 = CARTESIAN_POINT ( 'NONE',  ( -27.13199227600000185, 40.71900643419999710, -144.3906906950000177 ) ) ;
#7347 = ORIENTED_EDGE ( 'NONE', *, *, #13135, .T. ) ;
#7348 = CARTESIAN_POINT ( 'NONE',  ( -21.15827341640166992, 35.11213290585252622, -148.0734965375279160 ) ) ;
#7349 = DIRECTION ( 'NONE',  ( -0.6459422414661292189, 0.7633862853691524286, 0.000000000000000000 ) ) ;
#7350 = MECHANICAL_DESIGN_GEOMETRIC_PRESENTATION_REPRESENTATION (  '', ( #2425 ), #15705 ) ;
#7351 = ORIENTED_EDGE ( 'NONE', *, *, #21266, .T. ) ;
#7352 = APPLICATION_PROTOCOL_DEFINITION ( 'draft international standard', 'automotive_design', 1998, #14809 ) ;
#7353 = ORIENTED_EDGE ( 'NONE', *, *, #22760, .T. ) ;
#7354 = CARTESIAN_POINT ( 'NONE',  ( -12.50000000000000000, 45.50000000000000000, -151.0552959529999839 ) ) ;
#7355 = ADVANCED_FACE ( 'NONE', ( #9953 ), #6047, .F. ) ;
#7356 = CARTESIAN_POINT ( 'NONE',  ( 6.841811532420000397, -13.03968765259999962, -144.5552959529999839 ) ) ;
#7357 = CARTESIAN_POINT ( 'NONE',  ( 5.631397321050000571, -17.85059010000000157, -146.5552959529999839 ) ) ;
#7358 = ADVANCED_FACE ( 'NONE', ( #8050, #20800 ), #15435, .F. ) ;
#7359 = FACE_OUTER_BOUND ( 'NONE', #15769, .T. ) ;
#7360 = FACE_OUTER_BOUND ( 'NONE', #21658, .T. ) ;
#7361 = ORIENTED_EDGE ( 'NONE', *, *, #14812, .T. ) ;
#7362 = CARTESIAN_POINT ( 'NONE',  ( -13.04270098970000014, 34.92521805810000046, -147.0831430689999877 ) ) ;
#7363 = ADVANCED_FACE ( 'NONE', ( #9481 ), #20569, .F. ) ;
#7364 = LINE ( 'NONE', #465, #14797 ) ;
#7365 = ADVANCED_FACE ( 'NONE', ( #15216 ), #14974, .T. ) ;
#7366 = VERTEX_POINT ( 'NONE', #9710 ) ;
#7367 = DIRECTION ( 'NONE',  ( 1.000000000000000000, 0.000000000000000000, 0.000000000000000000 ) ) ;
#7368 = EDGE_CURVE ( 'NONE', #13630, #15489, #16986, .T. ) ;
#7369 = DIRECTION ( 'NONE',  ( 1.000000000000000000, 0.000000000000000000, -2.257018101830000309E-12 ) ) ;
#7370 = PLANE ( 'NONE',  #15868 ) ;
#7371 = CARTESIAN_POINT ( 'NONE',  ( -22.72559961389999827, 32.84666773589999877, -144.4841142160000231 ) ) ;
#7372 = VERTEX_POINT ( 'NONE', #11615 ) ;
#7373 = DIRECTION ( 'NONE',  ( -1.701177084980000217E-20, -4.426606872460000157E-37, -1.000000000000000000 ) ) ;
#7374 = CARTESIAN_POINT ( 'NONE',  ( -33.50000000000000000, 76.00000000000000000, -155.5552959529999839 ) ) ;
#7375 = CARTESIAN_POINT ( 'NONE',  ( 23.84377886109999878, -30.60602870049999780, -144.5552959529999839 ) ) ;
#7376 = CARTESIAN_POINT ( 'NONE',  ( -8.857008087982999101, -12.44928454996512635, -146.5552959529661621 ) ) ;
#7377 = FACE_OUTER_BOUND ( 'NONE', #9581, .T. ) ;
#7378 = CARTESIAN_POINT ( 'NONE',  ( -15.50000000000000000, 21.50000000000000000, -137.0552959530000123 ) ) ;
#7379 = EDGE_LOOP ( 'NONE', ( #5208, #21850, #12497, #18957 ) ) ;
#7380 = LINE ( 'NONE', #5120, #17148 ) ;
#7381 = LINE ( 'NONE', #16195, #13701 ) ;
#7382 = CARTESIAN_POINT ( 'NONE',  ( 7.500000000000002665, -3.892699081698711705, -150.0552959529999839 ) ) ;
#7383 = CARTESIAN_POINT ( 'NONE',  ( -5.810489697651222585, 41.13568347802100078, -141.5859922120193914 ) ) ;
#7384 = CARTESIAN_POINT ( 'NONE',  ( -13.49999999999999645, -43.19634954084936140, -136.0552959530033945 ) ) ;
#7385 = ORIENTED_EDGE ( 'NONE', *, *, #9407, .T. ) ;
#7386 = VECTOR ( 'NONE', #6942, 1000.000000000000000 ) ;
#7387 = DIRECTION ( 'NONE',  ( 1.000000000000000000, 2.602084704489999637E-17, -1.701177084830000066E-20 ) ) ;
#7388 = PLANE ( 'NONE',  #4883 ) ;
#7389 = VERTEX_POINT ( 'NONE', #2600 ) ;
#7390 = PRODUCT_DEFINITION_SHAPE ( 'NONE', 'NONE',  #10930 ) ;
#7391 = ADVANCED_FACE ( 'NONE', ( #9829 ), #17108, .T. ) ;
#7392 = ORIENTED_EDGE ( 'NONE', *, *, #18810, .F. ) ;
#7393 = CARTESIAN_POINT ( 'NONE',  ( -32.50000000000000000, -43.00000000050000182, -137.0552959530000123 ) ) ;
#7394 = CARTESIAN_POINT ( 'NONE',  ( 1.000000000160000013, 41.50000000000000000, -140.0552959529999839 ) ) ;
#7395 = FACE_OUTER_BOUND ( 'NONE', #22104, .T. ) ;
#7396 = DIRECTION ( 'NONE',  ( 1.000000000000000000, 0.000000000000000000, 0.000000000000000000 ) ) ;
#7397 = VERTEX_POINT ( 'NONE', #10864 ) ;
#7398 = CARTESIAN_POINT ( 'NONE',  ( -10.15741051819999896, 33.19655140199999721, -141.5761258080000005 ) ) ;
#7399 = CARTESIAN_POINT ( 'NONE',  ( -18.28451977777580240, 36.23520409085267602, -147.6763998119407972 ) ) ;
#7400 = CARTESIAN_POINT ( 'NONE',  ( 31.00000000000000000, -39.80430157320000006, -149.5552959529999839 ) ) ;
#7401 = DIRECTION ( 'NONE',  ( -3.994014902950000436E-29, 1.000000000000000000, -4.148443855749999753E-27 ) ) ;
#7402 = CARTESIAN_POINT ( 'NONE',  ( -22.73109880832327789, 38.77532135884324305, -140.2559096066406141 ) ) ;
#7403 = CARTESIAN_POINT ( 'NONE',  ( -34.50000000000000000, 47.00000000000000000, -146.5552959529999839 ) ) ;
#7404 = DIRECTION ( 'NONE',  ( 0.000000000000000000, 0.000000000000000000, 1.000000000000000000 ) ) ;
#7405 = FACE_OUTER_BOUND ( 'NONE', #9854, .T. ) ;
#7406 = CARTESIAN_POINT ( 'NONE',  ( 32.50000000000000000, -36.53620104889999709, -136.0552959530000123 ) ) ;
#7407 = VERTEX_POINT ( 'NONE', #21605 ) ;
#7408 = CARTESIAN_POINT ( 'NONE',  ( -5.992616235259950130, 37.70616357870241586, -147.6478618792677366 ) ) ;
#7409 = VERTEX_POINT ( 'NONE', #17913 ) ;
#7410 = EDGE_CURVE ( 'NONE', #11085, #20880, #11976, .T. ) ;
#7411 = SURFACE_STYLE_FILL_AREA ( #11200 ) ;
#7412 = ADVANCED_FACE ( 'NONE', ( #19241 ), #12539, .T. ) ;
#7413 = FACE_OUTER_BOUND ( 'NONE', #13734, .T. ) ;
#7415 = VECTOR ( 'NONE', #4647, 1000.000000000000000 ) ;
#7414 = DIRECTION ( 'NONE',  ( 1.000000000000000000, 0.000000000000000000, 0.000000000000000000 ) ) ;
#7416 = EDGE_CURVE ( 'NONE', #11512, #21536, #21578, .T. ) ;
#7417 = DIRECTION ( 'NONE',  ( 0.000000000000000000, 0.000000000000000000, 1.000000000000000000 ) ) ;
#7418 = PLANE ( 'NONE',  #7080 ) ;
#7419 = COLOUR_RGB ( '', 0.09019608, 0.27058824, 0.51372549) ;
#7420 = DIRECTION ( 'NONE',  ( 2.507771768019999718E-12, 1.592654864209999947E-17, -1.000000000000000000 ) ) ;
#7421 = ITEM_DEFINED_TRANSFORMATION ( 'NONE', 'NONE', #7711,  #5025 ) ;
#7422 = CARTESIAN_POINT ( 'NONE',  ( 6.750000000000000000, -47.00000000000000000, -150.0552959529999839 ) ) ;
#7423 = DIRECTION ( 'NONE',  ( -1.000000000000000000, 0.000000000000000000, 0.000000000000000000 ) ) ;
#7424 = CARTESIAN_POINT ( 'NONE',  ( -32.50000000000000000, -50.50000000000000000, -136.5552959530000123 ) ) ;
#7425 = ORIENTED_EDGE ( 'NONE', *, *, #18621, .F. ) ;
#7426 = ORIENTED_EDGE ( 'NONE', *, *, #7168, .T. ) ;
#7427 = ORIENTED_EDGE ( 'NONE', *, *, #2686, .F. ) ;
#7428 = FACE_OUTER_BOUND ( 'NONE', #14560, .T. ) ;
#7429 = ORIENTED_EDGE ( 'NONE', *, *, #78, .T. ) ;
#7430 = AXIS2_PLACEMENT_3D ( 'NONE', #9569, #9792, #555 ) ;
#7431 = CARTESIAN_POINT ( 'NONE',  ( 25.00000000000000000, -20.50000000000000000, -137.0552959530000123 ) ) ;
#7432 = ORIENTED_EDGE ( 'NONE', *, *, #307, .T. ) ;
#7433 = DIRECTION ( 'NONE',  ( -0.9892101392001054760, 0.1465035852930155480, 4.471489433380478225E-12 ) ) ;
#7434 = CARTESIAN_POINT ( 'NONE',  ( -20.34334609172888264, 35.37018562970122559, -140.7073119323060268 ) ) ;
#7435 = LINE ( 'NONE', #14698, #20093 ) ;
#7436 = VERTEX_POINT ( 'NONE', #16363 ) ;
#7437 = FACE_BOUND ( 'NONE', #13944, .T. ) ;
#7438 = EDGE_CURVE ( 'NONE', #4564, #10851, #18154, .T. ) ;
#7439 = LINE ( 'NONE', #14702, #12107 ) ;
#7440 = ADVANCED_FACE ( 'NONE', ( #7077 ), #22824, .F. ) ;
#7441 = CARTESIAN_POINT ( 'NONE',  ( 6.500000000130000011, 20.50000000000000000, -150.5552959529999839 ) ) ;
#7442 = CIRCLE ( 'NONE', #21134, 7.499999999999999112 ) ;
#7443 = DIRECTION ( 'NONE',  ( 1.000000000000000000, 0.000000000000000000, 0.000000000000000000 ) ) ;
#7444 = AXIS2_PLACEMENT_3D ( 'NONE', #12384, #1245, #15736 ) ;
#7445 = EDGE_LOOP ( 'NONE', ( #3089, #11834, #10733, #12920 ) ) ;
#7446 = PLANE ( 'NONE',  #12201 ) ;
#7447 = ORIENTED_EDGE ( 'NONE', *, *, #21957, .T. ) ;
#7448 = CARTESIAN_POINT ( 'NONE',  ( -12.50000000000000000, 19.50000000000000000, -136.5552959530000123 ) ) ;
#7449 = VERTEX_POINT ( 'NONE', #5290 ) ;
#7450 = CARTESIAN_POINT ( 'NONE',  ( -26.63329978995851022, 40.09797676221232621, -142.2284921075155921 ) ) ;
#7451 = VERTEX_POINT ( 'NONE', #3630 ) ;
#7452 = CARTESIAN_POINT ( 'NONE',  ( -22.52780672250980132, 37.05898997718779952, -140.0074087194032018 ) ) ;
#7453 = ORIENTED_EDGE ( 'NONE', *, *, #5055, .T. ) ;
#7454 = CARTESIAN_POINT ( 'NONE',  ( 4.499999999879999102, -1.500000000000000000, -143.0552959529999839 ) ) ;
#7455 = EDGE_LOOP ( 'NONE', ( #11520, #20571, #15880, #22113 ) ) ;
#7456 = CARTESIAN_POINT ( 'NONE',  ( -17.94987361340509580, -38.12165543836343318, -0.2372385574429291821 ) ) ;
#7457 = EDGE_CURVE ( 'NONE', #6756, #19314, #19129, .T. ) ;
#7458 = ORIENTED_EDGE ( 'NONE', *, *, #8925, .F. ) ;
#7459 = DIRECTION ( 'NONE',  ( 0.000000000000000000, 1.000000000000000000, 0.000000000000000000 ) ) ;
#7460 = CARTESIAN_POINT ( 'NONE',  ( -8.208807763370000288, 34.49436158469999469, -140.8229124829999819 ) ) ;
#7461 = VECTOR ( 'NONE', #8312, 1000.000000000000000 ) ;
#7462 = CARTESIAN_POINT ( 'NONE',  ( -32.50000000000000000, -35.00000000000000000, -151.0552959529999839 ) ) ;
#7463 = CARTESIAN_POINT ( 'NONE',  ( -6.565507373411123559, 37.00519331013514801, -148.7410818962522114 ) ) ;
#7464 = DIRECTION ( 'NONE',  ( -2.839308199620000013E-14, -3.568879590630000244E-13, -1.000000000000000000 ) ) ;
#7465 = LINE ( 'NONE', #22112, #15536 ) ;
#7466 = ORIENTED_EDGE ( 'NONE', *, *, #810, .T. ) ;
#7467 = DIRECTION ( 'NONE',  ( -4.430233957459999899E-12, 6.110667527539999876E-13, -1.000000000000000000 ) ) ;
#7468 = EDGE_CURVE ( 'NONE', #3293, #5505, #8848, .T. ) ;
#7469 = CARTESIAN_POINT ( 'NONE',  ( 25.50000000000000000, 22.50000000000000000, -150.0552959529999839 ) ) ;
#7470 = VERTEX_POINT ( 'NONE', #2951 ) ;
#7471 = FACE_OUTER_BOUND ( 'NONE', #6009, .T. ) ;
#7472 = CARTESIAN_POINT ( 'NONE',  ( -20.75825067126470813, -4.460833112886678720, -146.3157682190060029 ) ) ;
#7473 = EDGE_CURVE ( 'NONE', #22736, #18669, #2832, .T. ) ;
#7474 = CARTESIAN_POINT ( 'NONE',  ( -17.02285281771896308, 37.95643371699240731, -139.4648240190154524 ) ) ;
#7475 = CARTESIAN_POINT ( 'NONE',  ( -29.00775545215896400, 40.69683423424014990, -142.7914494781169026 ) ) ;
#7476 = CIRCLE ( 'NONE', #1420, 0.7500000000000006661 ) ;
#7477 = VERTEX_POINT ( 'NONE', #1857 ) ;
#7478 = CARTESIAN_POINT ( 'NONE',  ( 18.95053822279999878, 50.00000000000000000, -149.5552959529999839 ) ) ;
#7479 = CYLINDRICAL_SURFACE ( 'NONE', #12762, 0.7500000000000006661 ) ;
#7480 = DIRECTION ( 'NONE',  ( 1.000000000000000000, 0.000000000000000000, 0.000000000000000000 ) ) ;
#7481 = DIRECTION ( 'NONE',  ( -0.000000000000000000, 1.000000000000000000, 0.000000000000000000 ) ) ;
#7482 = CARTESIAN_POINT ( 'NONE',  ( 5.219138307789999764, -2.183626157169999971, -143.0552959529999839 ) ) ;
#7483 = DIRECTION ( 'NONE',  ( 0.6459422414661292189, 0.7633862853691524286, 2.257144641400453113E-12 ) ) ;
#7484 = CARTESIAN_POINT ( 'NONE',  ( -20.49362533948273679, 38.90000993910273763, -139.7618038651926327 ) ) ;
#7485 = ORIENTED_EDGE ( 'NONE', *, *, #14647, .T. ) ;
#7486 = CARTESIAN_POINT ( 'NONE',  ( 6.000000000140000012, 29.48610037779999971, -147.0552959529999839 ) ) ;
#7487 = ADVANCED_FACE ( 'NONE', ( #21728 ), #18028, .T. ) ;
#7488 = DIRECTION ( 'NONE',  ( 1.000000000000000000, 0.000000000000000000, -2.257453483404482811E-12 ) ) ;
#7489 = CARTESIAN_POINT ( 'NONE',  ( 2.048233066679999936, -63.64014441970000746, -143.0552959529999839 ) ) ;
#7490 = EDGE_CURVE ( 'NONE', #5244, #20874, #12415, .T. ) ;
#7491 = DIRECTION ( 'NONE',  ( 1.000000000000000000, 0.000000000000000000, 0.000000000000000000 ) ) ;
#7492 = DIRECTION ( 'NONE',  ( -1.000000000000000000, 0.000000000000000000, -2.245315044999999693E-12 ) ) ;
#7493 = EDGE_CURVE ( 'NONE', #2813, #9406, #8259, .T. ) ;
#7494 = AXIS2_PLACEMENT_3D ( 'NONE', #8963, #1184, #1740 ) ;
#7495 = VERTEX_POINT ( 'NONE', #6958 ) ;
#7496 = DIRECTION ( 'NONE',  ( -0.000000000000000000, 1.000000000000000000, 0.000000000000000000 ) ) ;
#7497 = EDGE_CURVE ( 'NONE', #13760, #18415, #9783, .T. ) ;
#7498 = AXIS2_PLACEMENT_3D ( 'NONE', #11677, #16697, #412 ) ;
#7499 = CARTESIAN_POINT ( 'NONE',  ( -9.434278515689999978, -18.41834002140000237, -147.5552959529999839 ) ) ;
#7500 = ORIENTED_EDGE ( 'NONE', *, *, #4756, .F. ) ;
#7501 = EDGE_LOOP ( 'NONE', ( #16046, #11848, #6566, #9929 ) ) ;
#7502 = PLANE ( 'NONE',  #8198 ) ;
#7503 = LINE ( 'NONE', #10948, #19996 ) ;
#7504 = CARTESIAN_POINT ( 'NONE',  ( -21.33871772390000032, 34.54066873269999860, -147.2646375960000000 ) ) ;
#7505 = CARTESIAN_POINT ( 'NONE',  ( 7.661661249388155071, 35.75613975769173436, -141.8866982259418137 ) ) ;
#7506 = ORIENTED_EDGE ( 'NONE', *, *, #18836, .F. ) ;
#7507 = CARTESIAN_POINT ( 'NONE',  ( -9.394779979509999990, -17.86685386420000299, -143.5552959529999839 ) ) ;
#7508 = CARTESIAN_POINT ( 'NONE',  ( -18.08440866526200352, 35.37133319620465954, -147.7332747159482551 ) ) ;
#7509 = VECTOR ( 'NONE', #22388, 1000.000000000000000 ) ;
#7510 = CARTESIAN_POINT ( 'NONE',  ( 24.59017985859999911, -26.91621017459999976, -148.5552959529999839 ) ) ;
#7511 = CARTESIAN_POINT ( 'NONE',  ( -22.62924774399843741, 37.91877106612172099, -140.0196664482663778 ) ) ;
#7512 = VECTOR ( 'NONE', #9484, 1000.000000000000114 ) ;
#7513 = CARTESIAN_POINT ( 'NONE',  ( 8.250000000030000891, -37.98606797749999942, -137.0552959530000123 ) ) ;
#7514 = EDGE_CURVE ( 'NONE', #4286, #1507, #21044, .T. ) ;
#7515 = DIRECTION ( 'NONE',  ( -1.000000000000000000, 1.156482317317871725E-15, 0.000000000000000000 ) ) ;
#7516 = DIRECTION ( 'NONE',  ( 0.000000000000000000, 0.000000000000000000, 1.000000000000000000 ) ) ;
#7517 = CARTESIAN_POINT ( 'NONE',  ( -9.969904307360000217, -22.67446893780000039, -145.5552959529999839 ) ) ;
#7518 = ORIENTED_EDGE ( 'NONE', *, *, #5188, .F. ) ;
#7519 = DIRECTION ( 'NONE',  ( 0.000000000000000000, 0.000000000000000000, 1.000000000000000000 ) ) ;
#7520 = EDGE_LOOP ( 'NONE', ( #9885, #6034 ) ) ;
#7521 = CARTESIAN_POINT ( 'NONE',  ( -2.499999999959999997, 34.00000000000000000, -136.0552959530000123 ) ) ;
#7522 = VECTOR ( 'NONE', #19177, 1000.000000000000000 ) ;
#7523 = CARTESIAN_POINT ( 'NONE',  ( -6.320468577110000652, -16.70961797440000041, -146.5552959529999839 ) ) ;
#7524 = VECTOR ( 'NONE', #13502, 1000.000000000000000 ) ;
#7525 = CARTESIAN_POINT ( 'NONE',  ( 13.13369214859999978, -51.00000000000000000, -136.0552959530000123 ) ) ;
#7526 = CARTESIAN_POINT ( 'NONE',  ( -24.22314457578830016, 36.96432676147898633, -148.6204621725165964 ) ) ;
#7527 = CARTESIAN_POINT ( 'NONE',  ( -13.10382330435357190, 34.73913613269233736, -140.9738839404401460 ) ) ;
#7528 = DIRECTION ( 'NONE',  ( 5.094701932209999624E-24, 1.000000000000000000, -1.149947916579999802E-35 ) ) ;
#7529 = CARTESIAN_POINT ( 'NONE',  ( 13.09808825513362862, 34.66051412330866555, -150.0552959529999839 ) ) ;
#7530 = LINE ( 'NONE', #4089, #5220 ) ;
#7531 = CARTESIAN_POINT ( 'NONE',  ( -34.50000000000000000, 0.9999999999959999775, -132.5552959530000123 ) ) ;
#7532 = LINE ( 'NONE', #22416, #12841 ) ;
#7533 = ORIENTED_EDGE ( 'NONE', *, *, #2855, .T. ) ;
#7535 = ORIENTED_EDGE ( 'NONE', *, *, #4379, .T. ) ;
#7534 = VECTOR ( 'NONE', #17393, 1000.000000000000000 ) ;
#7536 =( LENGTH_UNIT ( ) NAMED_UNIT ( * ) SI_UNIT ( .MILLI., .METRE. ) );
#7537 = VECTOR ( 'NONE', #22939, 1000.000000000000000 ) ;
#7538 = EDGE_CURVE ( 'NONE', #7205, #22524, #15684, .T. ) ;
#7539 = VECTOR ( 'NONE', #974, 1000.000000000000000 ) ;
#7540 = VERTEX_POINT ( 'NONE', #23382 ) ;
#7541 = CARTESIAN_POINT ( 'NONE',  ( -13.37538095157338880, 35.38499319558606970, -148.0468720929505082 ) ) ;
#7542 = DIRECTION ( 'NONE',  ( 0.000000000000000000, 1.000000000000000000, 0.000000000000000000 ) ) ;
#7543 = DIRECTION ( 'NONE',  ( -0.6459422414661292189, -0.7633862853691524286, 1.457985068980290749E-12 ) ) ;
#7544 = AXIS2_PLACEMENT_3D ( 'NONE', #19735, #1544, #18063 ) ;
#7545 = VERTEX_POINT ( 'NONE', #23265 ) ;
#7546 = AXIS2_PLACEMENT_3D ( 'NONE', #22495, #6189, #22257 ) ;
#7547 = CARTESIAN_POINT ( 'NONE',  ( 6.841811532410000396, -13.03968765259999962, -145.5552959529999839 ) ) ;
#7548 = LINE ( 'NONE', #20410, #19385 ) ;
#7549 = DIRECTION ( 'NONE',  ( -0.1736481776649230202, 0.000000000000000000, 0.9848077530125619594 ) ) ;
#7550 = ORIENTED_EDGE ( 'NONE', *, *, #784, .T. ) ;
#7551 = CARTESIAN_POINT ( 'NONE',  ( -19.69393976287956249, 37.84845892294580239, -140.3168504267079868 ) ) ;
#7552 = CARTESIAN_POINT ( 'NONE',  ( 9.151339728411230112, 38.35153067472349875, -141.9520366269342446 ) ) ;
#7553 = VECTOR ( 'NONE', #18883, 1000.000000000000000 ) ;
#7554 = DIRECTION ( 'NONE',  ( 1.000000000000000000, 0.000000000000000000, 0.000000000000000000 ) ) ;
#7555 = CIRCLE ( 'NONE', #11726, 1.500000000000001332 ) ;
#7556 = DIRECTION ( 'NONE',  ( -2.257144641399999941E-12, 0.000000000000000000, -1.000000000000000000 ) ) ;
#7557 = ORIENTED_EDGE ( 'NONE', *, *, #6924, .F. ) ;
#7558 = CIRCLE ( 'NONE', #12881, 1.499999999999999556 ) ;
#7559 = AXIS2_PLACEMENT_3D ( 'NONE', #13641, #17449, #1177 ) ;
#7560 = CARTESIAN_POINT ( 'NONE',  ( -32.50000000000000000, -1.000000000000000000, -145.5552959529999839 ) ) ;
#7561 = EDGE_LOOP ( 'NONE', ( #16203, #4861, #17002, #4205 ) ) ;
#7562 = DIRECTION ( 'NONE',  ( 0.7633862853691523176, -0.6459422414661291079, 0.000000000000000000 ) ) ;
#7563 = VERTEX_POINT ( 'NONE', #19691 ) ;
#7564 = CARTESIAN_POINT ( 'NONE',  ( -26.19677859571902445, 41.24837624377309453, -144.5491401104135605 ) ) ;
#7565 = EDGE_LOOP ( 'NONE', ( #15686, #6651, #324, #13795, #7114, #1051 ) ) ;
#7566 = EDGE_CURVE ( 'NONE', #12438, #13908, #18414, .T. ) ;
#7567 = CARTESIAN_POINT ( 'NONE',  ( -22.01591886049312308, 32.20669244871583459, -144.4616323330807290 ) ) ;
#7568 = EDGE_LOOP ( 'NONE', ( #14582, #3544, #17746, #10892 ) ) ;
#7569 = CARTESIAN_POINT ( 'NONE',  ( 4.500000000000000000, -3.500000000000000000, -140.0552959529999839 ) ) ;
#7570 = ADVANCED_FACE ( 'NONE', ( #16582 ), #18486, .T. ) ;
#7571 = ORIENTED_EDGE ( 'NONE', *, *, #8062, .F. ) ;
#7572 = VECTOR ( 'NONE', #15024, 1000.000000000000000 ) ;
#7573 = ORIENTED_EDGE ( 'NONE', *, *, #8183, .F. ) ;
#7574 = CARTESIAN_POINT ( 'NONE',  ( -25.85824191589999899, -1.500000000000000000, -145.5657682190000060 ) ) ;
#7575 = VECTOR ( 'NONE', #8229, 1000.000000000000000 ) ;
#7576 = LINE ( 'NONE', #7804, #17852 ) ;
#7577 = CARTESIAN_POINT ( 'NONE',  ( 13.95201674008764137, 21.48075934361423478, -150.0552959530000123 ) ) ;
#7578 = DIRECTION ( 'NONE',  ( 2.839308199620000013E-14, 3.568879590630000244E-13, 1.000000000000000000 ) ) ;
#7579 = VECTOR ( 'NONE', #2711, 1000.000000000000114 ) ;
#7580 = DIRECTION ( 'NONE',  ( -1.211690350418039921E-27, -2.765629237168040089E-27, 1.000000000000000000 ) ) ;
#7581 = AXIS2_PLACEMENT_3D ( 'NONE', #18785, #7940, #15224 ) ;
#7582 = CARTESIAN_POINT ( 'NONE',  ( -32.00000000000000000, -36.00000000000000000, -137.0552959530000123 ) ) ;
#7583 = VECTOR ( 'NONE', #19393, 999.9999999999998863 ) ;
#7584 = ORIENTED_EDGE ( 'NONE', *, *, #10838, .T. ) ;
#7585 = DIRECTION ( 'NONE',  ( 1.000000000000000000, 0.000000000000000000, 2.516505522483685870E-12 ) ) ;
#7586 = FACE_OUTER_BOUND ( 'NONE', #3059, .T. ) ;
#7587 = ORIENTED_EDGE ( 'NONE', *, *, #12709, .T. ) ;
#7588 = CARTESIAN_POINT ( 'NONE',  ( 14.79224200840030257, -34.50000000000000000, -149.4708568728852356 ) ) ;
#7589 = CARTESIAN_POINT ( 'NONE',  ( -11.58731752069515863, 38.53682247841263830, -140.5940415739001708 ) ) ;
#7590 = CARTESIAN_POINT ( 'NONE',  ( -16.91592704284670035, 37.75347730502732446, -140.5160138913198011 ) ) ;
#7591 = CARTESIAN_POINT ( 'NONE',  ( -29.62481956335792788, 40.87340935592879276, -146.3463541502384544 ) ) ;
#7592 = ORIENTED_EDGE ( 'NONE', *, *, #20887, .T. ) ;
#7593 = SURFACE_SIDE_STYLE ('',( #3925 ) ) ;
#7594 = DIRECTION ( 'NONE',  ( -3.994014902950000436E-29, 1.000000000000000000, -4.148443855750100198E-27 ) ) ;
#7595 = VECTOR ( 'NONE', #2561, 1000.000000000000000 ) ;
#7596 = ORIENTED_EDGE ( 'NONE', *, *, #1533, .T. ) ;
#7597 = LINE ( 'NONE', #10805, #1156 ) ;
#7598 = PLANE ( 'NONE',  #20222 ) ;
#7599 = AXIS2_PLACEMENT_3D ( 'NONE', #7113, #8765, #7236 ) ;
#7600 = CARTESIAN_POINT ( 'NONE',  ( 7.750000000000000000, 0.000000000000000000, -150.0552959529999839 ) ) ;
#7601 = CARTESIAN_POINT ( 'NONE',  ( -20.11972240904378495, 41.31329007930804664, -143.7317463393834203 ) ) ;
#7602 = EDGE_CURVE ( 'NONE', #23428, #6865, #9661, .T. ) ;
#7603 = EDGE_LOOP ( 'NONE', ( #15226, #7587, #6759, #345, #2229, #20910, #4353, #7264 ) ) ;
#7604 = LINE ( 'NONE', #18553, #13740 ) ;
#7605 = DIRECTION ( 'NONE',  ( 0.000000000000000000, 0.000000000000000000, 1.000000000000000000 ) ) ;
#7606 = DIRECTION ( 'NONE',  ( 0.7739965043580748771, 0.6331898698190620012, -3.042011087472929325E-12 ) ) ;
#7607 = CARTESIAN_POINT ( 'NONE',  ( 19.13369214879999802, 50.49999999980000354, -143.0552959529999839 ) ) ;
#7608 = DIRECTION ( 'NONE',  ( 1.000000000000000000, 0.000000000000000000, -2.854859206178974232E-14 ) ) ;
#7609 = ORIENTED_EDGE ( 'NONE', *, *, #551, .T. ) ;
#7610 = DIRECTION ( 'NONE',  ( -1.000000000000000000, 0.000000000000000000, -2.516505522483685870E-12 ) ) ;
#7611 = EDGE_CURVE ( 'NONE', #13431, #4685, #20176, .T. ) ;
#7612 = FACE_OUTER_BOUND ( 'NONE', #13376, .T. ) ;
#7613 = EDGE_LOOP ( 'NONE', ( #15509, #21470, #21303, #15582 ) ) ;
#7614 = VECTOR ( 'NONE', #7143, 1000.000000000000000 ) ;
#7615 = VECTOR ( 'NONE', #14963, 1000.000000000000000 ) ;
#7616 = ORIENTED_EDGE ( 'NONE', *, *, #5999, .F. ) ;
#7617 = DIRECTION ( 'NONE',  ( 1.526468026909860048E-13, 8.159623473498529972E-13, 1.000000000000000000 ) ) ;
#7618 = EDGE_CURVE ( 'NONE', #11046, #13504, #16934, .T. ) ;
#7619 = CARTESIAN_POINT ( 'NONE',  ( -30.64259443220337786, 40.28463426600038133, -145.8661425198802988 ) ) ;
#7620 = EDGE_CURVE ( 'NONE', #6228, #22167, #16825, .T. ) ;
#7621 = PLANE ( 'NONE',  #17384 ) ;
#7622 = CARTESIAN_POINT ( 'NONE',  ( 7.431199231726023591, 35.94753734600692496, -141.7876273308503414 ) ) ;
#7623 = VERTEX_POINT ( 'NONE', #293 ) ;
#7624 = CARTESIAN_POINT ( 'NONE',  ( -18.17807444413858775, 34.66091580349097256, -147.3401956634381236 ) ) ;
#7625 = ADVANCED_FACE ( 'NONE', ( #20049 ), #9200, .F. ) ;
#7626 = DIRECTION ( 'NONE',  ( -1.211690350418039921E-27, -2.765629237168040089E-27, 1.000000000000000000 ) ) ;
#7627 = CARTESIAN_POINT ( 'NONE',  ( 13.98537695664809277, 33.88080765318336063, -136.0552959530315320 ) ) ;
#7628 = EDGE_CURVE ( 'NONE', #824, #12377, #3865, .T. ) ;
#7629 = CARTESIAN_POINT ( 'NONE',  ( -23.03778781513472040, 40.78628791076015858, -141.9896475656336179 ) ) ;
#7630 = AXIS2_PLACEMENT_3D ( 'NONE', #8522, #12568, #19494 ) ;
#7631 = CARTESIAN_POINT ( 'NONE',  ( -15.73345061033185210, 33.26188818293405802, -144.2173886784002548 ) ) ;
#7632 = DIRECTION ( 'NONE',  ( 8.955190032050000935E-12, -9.104778821549999739E-13, 1.000000000000000000 ) ) ;
#7633 = FACE_OUTER_BOUND ( 'NONE', #14373, .T. ) ;
#7634 = LINE ( 'NONE', #18821, #6994 ) ;
#7635 = ORIENTED_EDGE ( 'NONE', *, *, #20641, .T. ) ;
#7636 = CARTESIAN_POINT ( 'NONE',  ( -5.832642628619999492, 38.59814668869999821, -147.7665506369999662 ) ) ;
#7637 = CARTESIAN_POINT ( 'NONE',  ( 32.50000000000000000, -39.92025131119999770, -149.5552959529999839 ) ) ;
#7638 = EDGE_CURVE ( 'NONE', #11916, #1387, #10142, .T. ) ;
#7639 = ORIENTED_EDGE ( 'NONE', *, *, #5491, .T. ) ;
#7640 = EDGE_CURVE ( 'NONE', #3754, #10756, #7532, .T. ) ;
#7641 = DIRECTION ( 'NONE',  ( 1.526468026909655070E-13, 8.159623473495709763E-13, 1.000000000000000000 ) ) ;
#7642 = CARTESIAN_POINT ( 'NONE',  ( -22.36052286279805301, 33.87069800589680568, -145.8484948931464089 ) ) ;
#7643 = VECTOR ( 'NONE', #2763, 1000.000000000000000 ) ;
#7644 = DIRECTION ( 'NONE',  ( 0.000000000000000000, 0.000000000000000000, 1.000000000000000000 ) ) ;
#7645 = ORIENTED_EDGE ( 'NONE', *, *, #20346, .F. ) ;
#7646 = VECTOR ( 'NONE', #14173, 1000.000000000000000 ) ;
#7647 = CARTESIAN_POINT ( 'NONE',  ( -12.49728671969152494, 33.10632428298641372, -146.3897782398302923 ) ) ;
#7648 = ADVANCED_FACE ( 'NONE', ( #20285 ), #3979, .F. ) ;
#7649 = CARTESIAN_POINT ( 'NONE',  ( -32.50000000000000000, 0.000000000000000000, -150.0552959529999839 ) ) ;
#7650 = EDGE_CURVE ( 'NONE', #1168, #7247, #20397, .T. ) ;
#7651 = FACE_OUTER_BOUND ( 'NONE', #19126, .T. ) ;
#7652 = PLANE ( 'NONE',  #9752 ) ;
#7653 = DIRECTION ( 'NONE',  ( 1.000000000000000000, 2.602084704489999637E-17, -1.701177084830000066E-20 ) ) ;
#7654 = EDGE_CURVE ( 'NONE', #10634, #9455, #10931, .T. ) ;
#7655 = CARTESIAN_POINT ( 'NONE',  ( -13.86630785140000022, 50.50000000000000000, -136.0552959530000123 ) ) ;
#7656 = VERTEX_POINT ( 'NONE', #7655 ) ;
#7657 = DIRECTION ( 'NONE',  ( -4.430318231639999944E-12, 6.100259101500000139E-13, -1.000000000000000000 ) ) ;
#7658 = ORIENTED_EDGE ( 'NONE', *, *, #10463, .T. ) ;
#7659 = ORIENTED_EDGE ( 'NONE', *, *, #2129, .F. ) ;
#7660 = CARTESIAN_POINT ( 'NONE',  ( -13.91784526120884102, 35.46792342019083577, -140.7554205114054184 ) ) ;
#7661 = LINE ( 'NONE', #16942, #21754 ) ;
#7662 = AXIS2_PLACEMENT_3D ( 'NONE', #12873, #13221, #12995 ) ;
#7663 = PLANE ( 'NONE',  #14201 ) ;
#7664 = CIRCLE ( 'NONE', #6535, 5.000000000000000000 ) ;
#7665 = ORIENTED_EDGE ( 'NONE', *, *, #2567, .T. ) ;
#7666 = CARTESIAN_POINT ( 'NONE',  ( 22.50000000000000000, 33.50000000000000000, -136.0552959530000123 ) ) ;
#7667 = CARTESIAN_POINT ( 'NONE',  ( 7.000000000070000894, 37.00000000000000000, -138.5552959529999839 ) ) ;
#7668 = FACE_OUTER_BOUND ( 'NONE', #14207, .T. ) ;
#7669 = ORIENTED_EDGE ( 'NONE', *, *, #14763, .F. ) ;
#7670 = CARTESIAN_POINT ( 'NONE',  ( -21.22372860086487023, 38.99008670914216879, -146.8399696847710914 ) ) ;
#7671 = CARTESIAN_POINT ( 'NONE',  ( 9.744924853801363085, 37.83677071069875097, -141.6994869973544837 ) ) ;
#7672 = SHAPE_REPRESENTATION ( 'MAS-159', ( #6581, #23314, #1662, #10375, #17992, #16470, #14943, #10746, #146, #16842, #1291, #3552, #7711, #19895, #3179 ), #18747 ) ;
#7673 = EDGE_CURVE ( 'NONE', #22550, #2114, #2327, .T. ) ;
#7674 = CARTESIAN_POINT ( 'NONE',  ( -18.22769797923111668, 36.96487028399717900, -148.6596776398728537 ) ) ;
#7675 = EDGE_CURVE ( 'NONE', #12039, #19224, #17239, .T. ) ;
#7676 = CARTESIAN_POINT ( 'NONE',  ( -27.77832206610000298, 37.03059619289999915, -147.6270870419999710 ) ) ;
#7677 = EDGE_LOOP ( 'NONE', ( #19260, #13461, #8079, #17661 ) ) ;
#7678 = VECTOR ( 'NONE', #4168, 1000.000000000000000 ) ;
#7679 = FACE_OUTER_BOUND ( 'NONE', #10202, .T. ) ;
#7680 = ORIENTED_EDGE ( 'NONE', *, *, #14053, .T. ) ;
#7681 = EDGE_LOOP ( 'NONE', ( #15615, #6372, #19248, #4281 ) ) ;
#7682 = CARTESIAN_POINT ( 'NONE',  ( -26.79508209637365468, 40.49614020271001635, -143.6492312593390750 ) ) ;
#7683 = EDGE_LOOP ( 'NONE', ( #19102, #9478, #6967, #16496 ) ) ;
#7684 = CARTESIAN_POINT ( 'NONE',  ( -23.32853373970316468, 36.96341023006359450, -139.4571126576117024 ) ) ;
#7685 = ORIENTED_EDGE ( 'NONE', *, *, #6601, .T. ) ;
#7686 = CARTESIAN_POINT ( 'NONE',  ( -29.88845675159999971, 40.47687533140000227, -144.8298193859999969 ) ) ;
#7687 = EDGE_LOOP ( 'NONE', ( #22713, #13671, #18155, #18114, #5078, #7790, #976, #10524 ) ) ;
#7688 = SHAPE_DEFINITION_REPRESENTATION ( #9516, #14082 ) ;
#7689 = VERTEX_POINT ( 'NONE', #20993 ) ;
#7690 = CARTESIAN_POINT ( 'NONE',  ( -7.500000000000000000, 22.50000000000000000, -151.0552959529999839 ) ) ;
#7691 = LINE ( 'NONE', #17093, #14420 ) ;
#7692 = DIRECTION ( 'NONE',  ( -2.808280234682504769E-18, 1.000000000000000000, 1.592654863660134930E-17 ) ) ;
#7693 = CARTESIAN_POINT ( 'NONE',  ( -12.50000000000000000, 48.50000000000000000, -150.5552959529999839 ) ) ;
#7694 = AXIS2_PLACEMENT_3D ( 'NONE', #4319, #20850, #19062 ) ;
#7695 = CARTESIAN_POINT ( 'NONE',  ( 10.93320006080000084, 3.500000000000000000, -148.5552959529999839 ) ) ;
#7696 = CARTESIAN_POINT ( 'NONE',  ( -8.475885007274353455, 38.89800807253860881, -139.6558146860800207 ) ) ;
#7697 = VERTEX_POINT ( 'NONE', #19312 ) ;
#7698 = DIRECTION ( 'NONE',  ( 1.000000000000000000, 0.000000000000000000, -1.701177084980000217E-20 ) ) ;
#7699 = ADVANCED_FACE ( 'NONE', ( #6111 ), #21811, .F. ) ;
#7700 = EDGE_CURVE ( 'NONE', #954, #6667, #6693, .T. ) ;
#7701 = CARTESIAN_POINT ( 'NONE',  ( 8.327852746066881195, -18.10800434007730786, -146.5552959530281782 ) ) ;
#7702 = CARTESIAN_POINT ( 'NONE',  ( -16.35051508389999597, -34.50000000000000000, -147.0118839079999873 ) ) ;
#7703 = EDGE_CURVE ( 'NONE', #9187, #1380, #19441, .T. ) ;
#7704 = VERTEX_POINT ( 'NONE', #1603 ) ;
#7705 = CARTESIAN_POINT ( 'NONE',  ( 3.249999999879999990, -3.000000000000000000, -135.4552959529999896 ) ) ;
#7706 = CARTESIAN_POINT ( 'NONE',  ( -11.86981902993892035, 40.35288497610176250, -142.1893091613364106 ) ) ;
#7707 = DIRECTION ( 'NONE',  ( 5.094701932209999624E-24, 1.000000000000000000, 0.000000000000000000 ) ) ;
#7708 = CARTESIAN_POINT ( 'NONE',  ( -35.73252798949999942, 26.50000000000000000, -138.5552959529999839 ) ) ;
#7709 = ORIENTED_EDGE ( 'NONE', *, *, #16087, .T. ) ;
#7710 = LINE ( 'NONE', #18670, #2953 ) ;
#7711 = AXIS2_PLACEMENT_3D ( 'NONE', #5907, #327, #2364 ) ;
#7712 = CARTESIAN_POINT ( 'NONE',  ( -30.68396739435302223, 40.64794745105156437, -146.0701989576815549 ) ) ;
#7713 = ORIENTED_EDGE ( 'NONE', *, *, #4003, .F. ) ;
#7714 = CARTESIAN_POINT ( 'NONE',  ( -15.50000000000000000, 21.50000000000000000, -136.5552959530000123 ) ) ;
#7715 = DIRECTION ( 'NONE',  ( 2.257171095940000041E-12, 1.003664318210000046E-28, 1.000000000000000000 ) ) ;
#7716 = VERTEX_POINT ( 'NONE', #21348 ) ;
#7717 = CARTESIAN_POINT ( 'NONE',  ( 25.96278831570000278, 46.03148680980000051, -150.0552959529999839 ) ) ;
#7718 = CARTESIAN_POINT ( 'NONE',  ( -20.24766572715067525, 39.88812938375418327, -140.1838214082657146 ) ) ;
#7719 = EDGE_LOOP ( 'NONE', ( #19392, #11053, #3580, #19640 ) ) ;
#7720 =( LENGTH_UNIT ( ) NAMED_UNIT ( * ) SI_UNIT ( .MILLI., .METRE. ) );
#7721 = FACE_OUTER_BOUND ( 'NONE', #3192, .T. ) ;
#7722 = DIRECTION ( 'NONE',  ( 0.000000000000000000, 1.000000000000000000, 0.000000000000000000 ) ) ;
#7723 = VERTEX_POINT ( 'NONE', #14078 ) ;
#7724 = LINE ( 'NONE', #22251, #8688 ) ;
#7725 = DIRECTION ( 'NONE',  ( -1.000000000000000000, 0.000000000000000000, 2.256683728769999802E-12 ) ) ;
#7726 = ADVANCED_FACE ( 'NONE', ( #5039 ), #12279, .F. ) ;
#7727 = CARTESIAN_POINT ( 'NONE',  ( -5.499999999959999997, 44.50000000000000000, -136.0552959530000123 ) ) ;
#7728 = ORIENTED_EDGE ( 'NONE', *, *, #23341, .T. ) ;
#7729 = CARTESIAN_POINT ( 'NONE',  ( 11.55556760165677233, -19.99386613923380906, -148.5552959529999839 ) ) ;
#7730 = DIRECTION ( 'NONE',  ( 0.000000000000000000, 1.000000000000000000, 0.000000000000000000 ) ) ;
#7731 = ORIENTED_EDGE ( 'NONE', *, *, #3277, .T. ) ;
#7732 = EDGE_CURVE ( 'NONE', #10602, #19256, #17756, .T. ) ;
#7733 = VERTEX_POINT ( 'NONE', #6934 ) ;
#7734 = CARTESIAN_POINT ( 'NONE',  ( -22.29630802378710541, 35.55620207364702168, -140.5780526047887520 ) ) ;
#7735 = DIRECTION ( 'NONE',  ( 1.000000000000000000, 2.602084704489999637E-17, -2.257171095940000041E-12 ) ) ;
#7736 = LINE ( 'NONE', #37, #7872 ) ;
#7737 = CARTESIAN_POINT ( 'NONE',  ( 8.014315017057485946, 35.57994765775046631, -141.9976801201232490 ) ) ;
#7738 = ORIENTED_EDGE ( 'NONE', *, *, #1252, .T. ) ;
#7739 = CARTESIAN_POINT ( 'NONE',  ( 12.50000000020000002, 24.10555127549999810, -139.5552959529999839 ) ) ;
#7740 = PRODUCT_RELATED_PRODUCT_CATEGORY ( 'part', '', ( #15507 ) ) ;
#7741 = PLANE ( 'NONE',  #4870 ) ;
#7742 = CARTESIAN_POINT ( 'NONE',  ( -1.500000000000000000, 44.50000000000000000, -150.0552959529999839 ) ) ;
#7743 = CARTESIAN_POINT ( 'NONE',  ( -6.366307851450000221, 51.50000000000000000, -136.0552959530000123 ) ) ;
#7744 = ADVANCED_FACE ( 'NONE', ( #12389 ), #14195, .F. ) ;
#7745 = CARTESIAN_POINT ( 'NONE',  ( -15.68268784160000173, 36.02211616019999951, -148.5535485649999998 ) ) ;
#7746 = AXIS2_PLACEMENT_3D ( 'NONE', #21939, #11084, #1839 ) ;
#7747 = CARTESIAN_POINT ( 'NONE',  ( -16.36784392959527779, 33.86562477376711655, -142.0582287346993837 ) ) ;
#7748 = CARTESIAN_POINT ( 'NONE',  ( 31.32297112069999656, -40.18599471579999971, -150.0552959529999839 ) ) ;
#7749 = LINE ( 'NONE', #15133, #18316 ) ;
#7750 = CARTESIAN_POINT ( 'NONE',  ( -18.35824191589999899, -34.50000000000000000, -144.8157682189915931 ) ) ;
#7751 = EDGE_CURVE ( 'NONE', #20549, #18609, #4066, .T. ) ;
#7752 = ORIENTED_EDGE ( 'NONE', *, *, #13707, .T. ) ;
#7753 = CARTESIAN_POINT ( 'NONE',  ( -6.518342001254413987, 39.10550174654262179, -146.8501022327429268 ) ) ;
#7754 = FACE_BOUND ( 'NONE', #2355, .T. ) ;
#7755 = ORIENTED_EDGE ( 'NONE', *, *, #10283, .T. ) ;
#7756 = LINE ( 'NONE', #20161, #3843 ) ;
#7757 = CARTESIAN_POINT ( 'NONE',  ( -22.93117458072607207, 34.96482181345525930, -141.2446360092426971 ) ) ;
#7758 = EDGE_CURVE ( 'NONE', #16283, #6873, #16270, .T. ) ;
#7759 = LINE ( 'NONE', #13231, #5288 ) ;
#7760 = ORIENTED_EDGE ( 'NONE', *, *, #19619, .F. ) ;
#7761 = CARTESIAN_POINT ( 'NONE',  ( -12.95309207269206020, 35.58606224184668321, -147.4460499725167892 ) ) ;
#7762 = CARTESIAN_POINT ( 'NONE',  ( 32.50000000000000000, 32.96379895120000469, -136.5552959530000123 ) ) ;
#7763 = VECTOR ( 'NONE', #2050, 1000.000000000000114 ) ;
#7764 = CARTESIAN_POINT ( 'NONE',  ( 12.88080765318778731, 38.01462304345265153, -150.0552959529999839 ) ) ;
#7765 = LINE ( 'NONE', #2546, #8248 ) ;
#7766 = CARTESIAN_POINT ( 'NONE',  ( 12.82492181439999968, -17.92284828160000032, -146.5552959529999839 ) ) ;
#7767 = CARTESIAN_POINT ( 'NONE',  ( -13.73025257492642126, 37.03482478361185315, -140.6242165752722997 ) ) ;
#7768 = ADVANCED_FACE ( 'NONE', ( #3718 ), #18463, .F. ) ;
#7769 = VERTEX_POINT ( 'NONE', #3955 ) ;
#7770 = EDGE_CURVE ( 'NONE', #20679, #17230, #21595, .T. ) ;
#7771 = CARTESIAN_POINT ( 'NONE',  ( -27.80359210608580156, 32.89696731219263626, -146.3345487532673701 ) ) ;
#7772 = ORIENTED_EDGE ( 'NONE', *, *, #14244, .T. ) ;
#7773 = ORIENTED_EDGE ( 'NONE', *, *, #10084, .T. ) ;
#7774 = DIRECTION ( 'NONE',  ( 2.842170943040000002E-14, 3.552713678800000097E-13, 1.000000000000000000 ) ) ;
#7775 = DIRECTION ( 'NONE',  ( 0.000000000000000000, 4.009147065150000317E-51, -1.000000000000000000 ) ) ;
#7776 = ADVANCED_FACE ( 'NONE', ( #16450 ), #22157, .F. ) ;
#7777 = VERTEX_POINT ( 'NONE', #3839 ) ;
#7778 = DIRECTION ( 'NONE',  ( 1.000000000000000000, 0.000000000000000000, -8.955799065309598247E-12 ) ) ;
#7779 = CARTESIAN_POINT ( 'NONE',  ( -16.50000000000000000, -43.00000000000000000, -136.5552959530000123 ) ) ;
#7780 = EDGE_CURVE ( 'NONE', #14361, #802, #508, .T. ) ;
#7781 = AXIS2_PLACEMENT_3D ( 'NONE', #14035, #10338, #8545 ) ;
#7782 = VERTEX_POINT ( 'NONE', #14899 ) ;
#7783 = CARTESIAN_POINT ( 'NONE',  ( -20.82480350055617535, 40.41812776023138554, -143.7337601291241356 ) ) ;
#7784 = EDGE_CURVE ( 'NONE', #22167, #6301, #21973, .T. ) ;
#7785 = EDGE_CURVE ( 'NONE', #3040, #22250, #5503, .T. ) ;
#7786 = CARTESIAN_POINT ( 'NONE',  ( 9.337668468615847317, 38.24431173749859880, -141.8869580488046154 ) ) ;
#7787 = LINE ( 'NONE', #20308, #16984 ) ;
#7788 = EDGE_LOOP ( 'NONE', ( #21147, #8365, #2815, #9970 ) ) ;
#7789 = FACE_OUTER_BOUND ( 'NONE', #1327, .T. ) ;
#7790 = ORIENTED_EDGE ( 'NONE', *, *, #12513, .F. ) ;
#7791 = VECTOR ( 'NONE', #20867, 1000.000000000000114 ) ;
#7792 = FACE_OUTER_BOUND ( 'NONE', #14178, .T. ) ;
#7793 = CIRCLE ( 'NONE', #6666, 0.7500000000000006661 ) ;
#7794 = ORIENTED_EDGE ( 'NONE', *, *, #17409, .T. ) ;
#7795 = CARTESIAN_POINT ( 'NONE',  ( -25.65708489768155331, 38.56472069215177356, -140.6657235122787881 ) ) ;
#7796 = VERTEX_POINT ( 'NONE', #267 ) ;
#7797 = CARTESIAN_POINT ( 'NONE',  ( -23.24537173081721164, 34.37218318494526414, -140.4769510064934082 ) ) ;
#7798 = ORIENTED_EDGE ( 'NONE', *, *, #7675, .F. ) ;
#7799 = DIRECTION ( 'NONE',  ( 0.000000000000000000, 0.000000000000000000, -1.000000000000000000 ) ) ;
#7800 = ORIENTED_EDGE ( 'NONE', *, *, #21402, .F. ) ;
#7801 = ORIENTED_EDGE ( 'NONE', *, *, #6908, .F. ) ;
#7802 = PLANE ( 'NONE',  #20136 ) ;
#7803 = APPLICATION_CONTEXT ( 'automotive_design' ) ;
#7804 = CARTESIAN_POINT ( 'NONE',  ( -9.157754307299999397, -15.75963164970000108, -148.5552959529999839 ) ) ;
#7805 = EDGE_CURVE ( 'NONE', #4889, #8373, #9286, .T. ) ;
#7806 = DIRECTION ( 'NONE',  ( -1.000000000000000000, 0.000000000000000000, 0.000000000000000000 ) ) ;
#7807 = DIRECTION ( 'NONE',  ( 1.000000000000000000, 0.000000000000000000, -8.955534726494208689E-12 ) ) ;
#7808 =( BOUNDED_SURFACE ( )  B_SPLINE_SURFACE ( 5, 5, ( 
 ( #22641, #6572, #20987, #8109, #13836, #17166 ),
 ( #20740, #8574, #6222, #4677, #8226, #21100 ),
 ( #15382, #885, #4434, #15495, #10008, #19427 ),
 ( #4792, #11671, #8350, #12035, #19184, #15622 ),
 ( #18948, #6684, #19304, #3017, #10254, #22756 ),
 ( #17519, #9889, #1244, #6332, #8467, #2663 ),
 ( #13586, #20861, #6457, #15735, #22995, #13713 ),
 ( #13945, #21217, #4909, #12157, #21571, #23461 ),
 ( #3599, #14071, #12629, #3477, #7037, #18231 ),
 ( #1820, #21338, #12742, #1946, #3239, #20013 ),
 ( #10715, #12503, #21451, #9164, #17996, #1706 ),
 ( #10945, #5379, #17878, #3708, #5132, #12383 ) ),
 .UNSPECIFIED., .F., .F., .F. ) 
 B_SPLINE_SURFACE_WITH_KNOTS ( ( 6, 3, 3, 6 ),
 ( 6, 6 ),
 ( 0.000000000000000000, 4.509114667229999540, 8.972055907920001516, 13.39149027790000090 ),
 ( 1.570796326489795058, 3.141592653590000062 ),
 .UNSPECIFIED. ) 
 GEOMETRIC_REPRESENTATION_ITEM ( )  RATIONAL_B_SPLINE_SURFACE ( (
 ( 0.2500000000000000000, 0.2499999999611400014, 0.2999999999417100049, 0.3999999999222799696, 0.5999999999222800362, 1.000000000000000000),
 ( 0.2500000000000000000, 0.2499999999611400014, 0.2999999999417100049, 0.3999999999222799696, 0.5999999999222800362, 1.000000000000000000),
 ( 0.2500000000000000000, 0.2499999999611400014, 0.2999999999417100049, 0.3999999999222799696, 0.5999999999222800362, 1.000000000000000000),
 ( 0.2500000000000000000, 0.2499999999611400014, 0.2999999999417100049, 0.3999999999222799696, 0.5999999999222800362, 1.000000000000000000),
 ( 0.2500000000000000000, 0.2499999999611400014, 0.2999999999417100049, 0.3999999999222799696, 0.5999999999222800362, 1.000000000000000000),
 ( 0.2500000000000000000, 0.2499999999611400014, 0.2999999999417100049, 0.3999999999222799696, 0.5999999999222800362, 1.000000000000000000),
 ( 0.2500000000000000000, 0.2499999999611400014, 0.2999999999417100049, 0.3999999999222799696, 0.5999999999222800362, 1.000000000000000000),
 ( 0.2500000000000000000, 0.2499999999611400014, 0.2999999999417100049, 0.3999999999222799696, 0.5999999999222800362, 1.000000000000000000),
 ( 0.2500000000000000000, 0.2499999999611400014, 0.2999999999417100049, 0.3999999999222799696, 0.5999999999222800362, 1.000000000000000000),
 ( 0.2500000000000000000, 0.2499999999611400014, 0.2999999999417100049, 0.3999999999222799696, 0.5999999999222800362, 1.000000000000000000),
 ( 0.2500000000000000000, 0.2499999999611400014, 0.2999999999417100049, 0.3999999999222799696, 0.5999999999222800362, 1.000000000000000000),
 ( 0.2500000000000000000, 0.2499999999611400014, 0.2999999999417100049, 0.3999999999222799696, 0.5999999999222800362, 1.000000000000000000) ) ) 
 REPRESENTATION_ITEM ( '' )  SURFACE ( )  );
#7809 = CARTESIAN_POINT ( 'NONE',  ( 0.000000000000000000, 19.50000000000000000, -150.0552959529999839 ) ) ;
#7810 = DIRECTION ( 'NONE',  ( 1.000000000000000000, 0.000000000000000000, 0.000000000000000000 ) ) ;
#7811 = ORIENTED_EDGE ( 'NONE', *, *, #9768, .T. ) ;
#7812 = CARTESIAN_POINT ( 'NONE',  ( 17.66940543669999997, -18.68690163239999791, -145.0552959529999839 ) ) ;
#7813 = VECTOR ( 'NONE', #21901, 1000.000000000000000 ) ;
#7814 = VECTOR ( 'NONE', #886, 1000.000000000000000 ) ;
#7815 = LINE ( 'NONE', #22343, #14029 ) ;
#7816 = PLANE ( 'NONE',  #2263 ) ;
#7817 = ORIENTED_EDGE ( 'NONE', *, *, #20743, .T. ) ;
#7818 = CARTESIAN_POINT ( 'NONE',  ( -12.63906142178066538, 39.72050110283642255, -147.8595189120993894 ) ) ;
#7819 = CARTESIAN_POINT ( 'NONE',  ( -17.67542686956860720, 41.20418847383326266, -146.4439386566194514 ) ) ;
#7820 = CARTESIAN_POINT ( 'NONE',  ( 1.133692148550000001, 50.50000000000000000, -142.8052959529999839 ) ) ;
#7821 = ORIENTED_EDGE ( 'NONE', *, *, #6311, .F. ) ;
#7822 = CARTESIAN_POINT ( 'NONE',  ( -7.856058713298979868, 37.01980778203124345, -139.4032252964223630 ) ) ;
#7823 = DIRECTION ( 'NONE',  ( -0.000000000000000000, 1.000000000000000000, 0.000000000000000000 ) ) ;
#7824 = ORIENTED_EDGE ( 'NONE', *, *, #2109, .T. ) ;
#7825 = DIRECTION ( 'NONE',  ( -2.257144641399999941E-12, 8.049635416090000264E-35, -1.000000000000000000 ) ) ;
#7826 = CARTESIAN_POINT ( 'NONE',  ( -28.67645553090000021, 33.79622934780000065, -142.1760638819999940 ) ) ;
#7827 = VERTEX_POINT ( 'NONE', #20023 ) ;
#7828 = CARTESIAN_POINT ( 'NONE',  ( -4.020716686303631882, 46.44926652720589999, -150.0552959530000123 ) ) ;
#7829 = CARTESIAN_POINT ( 'NONE',  ( -21.41042584029257512, 41.06450079727203217, -146.4204638434819969 ) ) ;
#7830 = ORIENTED_EDGE ( 'NONE', *, *, #16868, .F. ) ;
#7831 = CARTESIAN_POINT ( 'NONE',  ( -3.499999999929999994, 34.00000000000000000, -138.0552959530000123 ) ) ;
#7832 = PLANE ( 'NONE',  #2324 ) ;
#7833 = ADVANCED_FACE ( 'NONE', ( #5843 ), #21819, .F. ) ;
#7834 = VERTEX_POINT ( 'NONE', #9523 ) ;
#7835 = CARTESIAN_POINT ( 'NONE',  ( -2.499999999839999987, 20.50000000000000000, -140.5552959529999839 ) ) ;
#7836 = DIRECTION ( 'NONE',  ( -1.000000000000000000, 0.000000000000000000, 2.273736754430000208E-12 ) ) ;
#7837 = DIRECTION ( 'NONE',  ( 0.000000000000000000, 0.000000000000000000, 1.000000000000000000 ) ) ;
#7838 = ORIENTED_EDGE ( 'NONE', *, *, #1127, .T. ) ;
#7839 = CARTESIAN_POINT ( 'NONE',  ( -34.50000000000000000, 68.45885107719999496, -142.3001308290000111 ) ) ;
#7840 = CARTESIAN_POINT ( 'NONE',  ( -2.273230205652897240, 46.10147512692442717, -136.0552959529948680 ) ) ;
#7841 = EDGE_LOOP ( 'NONE', ( #7830, #19843, #15165 ) ) ;
#7842 = VECTOR ( 'NONE', #19212, 1000.000000000000000 ) ;
#7843 = ORIENTED_EDGE ( 'NONE', *, *, #20945, .F. ) ;
#7844 = CARTESIAN_POINT ( 'NONE',  ( -20.60824191589623666, -32.00000000000000000, -146.3157682190056335 ) ) ;
#7845 = ADVANCED_FACE ( 'NONE', ( #16559 ), #7741, .F. ) ;
#7846 = DIRECTION ( 'NONE',  ( 0.000000000000000000, 0.000000000000000000, 1.000000000000000000 ) ) ;
#7847 = LINE ( 'NONE', #15467, #1432 ) ;
#7848 = CARTESIAN_POINT ( 'NONE',  ( 7.657860202850368836, 35.75870734630790793, -141.8852171074365174 ) ) ;
#7849 = ORIENTED_EDGE ( 'NONE', *, *, #3555, .T. ) ;
#7850 = CARTESIAN_POINT ( 'NONE',  ( -32.50000000000000000, -2.273736754430000208E-12, -136.0552959530000123 ) ) ;
#7851 = FACE_OUTER_BOUND ( 'NONE', #21094, .T. ) ;
#7852 = FACE_OUTER_BOUND ( 'NONE', #10185, .T. ) ;
#7853 = DIRECTION ( 'NONE',  ( 0.000000000000000000, 1.000000000000000000, 0.000000000000000000 ) ) ;
#7854 = CARTESIAN_POINT ( 'NONE',  ( -24.63187620858801807, 37.01311550629854707, -148.7335123083401243 ) ) ;
#7855 = LINE ( 'NONE', #3958, #11818 ) ;
#7856 = CIRCLE ( 'NONE', #10895, 9.999999999999998224 ) ;
#7857 = ADVANCED_FACE ( 'NONE', ( #21930 ), #12750, .T. ) ;
#7858 = CARTESIAN_POINT ( 'NONE',  ( -16.81794493326261986, 37.02435727938188137, -140.5111119823011734 ) ) ;
#7859 = AXIS2_PLACEMENT_3D ( 'NONE', #15030, #22068, #18483 ) ;
#7860 = CARTESIAN_POINT ( 'NONE',  ( -4.499999999929999994, 42.50000000000000000, -138.0552959530000123 ) ) ;
#7861 = CARTESIAN_POINT ( 'NONE',  ( -5.459597139290000456, 36.94776568910000236, -139.8191173760000083 ) ) ;
#7862 = EDGE_CURVE ( 'NONE', #18719, #18280, #14662, .T. ) ;
#7863 = CARTESIAN_POINT ( 'NONE',  ( 24.85988213910000155, -26.16224997189999968, -144.5552959529999839 ) ) ;
#7864 = ORIENTED_EDGE ( 'NONE', *, *, #10533, .F. ) ;
#7865 = CARTESIAN_POINT ( 'NONE',  ( -5.064279449469999861, 40.47653686799999662, -142.0698957560000224 ) ) ;
#7866 = CARTESIAN_POINT ( 'NONE',  ( 9.438695624090803094, -28.66738265459707691, -147.5552959529370582 ) ) ;
#7867 = ORIENTED_EDGE ( 'NONE', *, *, #8375, .T. ) ;
#7868 = CARTESIAN_POINT ( 'NONE',  ( -21.03694116380903978, 36.94210036639064043, -147.9486865822370021 ) ) ;
#7869 = CARTESIAN_POINT ( 'NONE',  ( -7.816799939239999162, 0.9999999999989999111, -149.3052959529999839 ) ) ;
#7870 = VERTEX_POINT ( 'NONE', #9398 ) ;
#7871 = CARTESIAN_POINT ( 'NONE',  ( -12.47876718462605616, 33.77260538731622574, -145.9764135834861065 ) ) ;
#7872 = VECTOR ( 'NONE', #9041, 999.9999999999998863 ) ;
#7873 = DIRECTION ( 'NONE',  ( 0.1720749717299729364, 0.9850838563818457017, -6.484322019408987829E-13 ) ) ;
#7874 = CIRCLE ( 'NONE', #9769, 1.000000000000000888 ) ;
#7875 = CARTESIAN_POINT ( 'NONE',  ( -42.28007584270000052, 45.00000000000000000, -143.7573642109999810 ) ) ;
#7876 = DIRECTION ( 'NONE',  ( -1.000000000000000000, 0.000000000000000000, 2.257495777610000006E-12 ) ) ;
#7877 = DIRECTION ( 'NONE',  ( -0.000000000000000000, 1.000000000000000000, 0.000000000000000000 ) ) ;
#7878 = EDGE_CURVE ( 'NONE', #21963, #3124, #5614, .T. ) ;
#7879 = DIRECTION ( 'NONE',  ( 0.000000000000000000, 1.000000000000000000, 0.000000000000000000 ) ) ;
#7880 = ORIENTED_EDGE ( 'NONE', *, *, #15499, .T. ) ;
#7881 = CYLINDRICAL_SURFACE ( 'NONE', #9239, 0.7499999999999997780 ) ;
#7882 = ORIENTED_EDGE ( 'NONE', *, *, #20439, .T. ) ;
#7883 = CARTESIAN_POINT ( 'NONE',  ( -14.37102166023024807, 35.04507042385125004, -139.9665150629348318 ) ) ;
#7884 = CARTESIAN_POINT ( 'NONE',  ( -12.50000000000000000, 22.50000000000000000, -151.0552959529999839 ) ) ;
#7885 = DIRECTION ( 'NONE',  ( 1.526468026909999897E-13, 8.159623473500000156E-13, 1.000000000000000000 ) ) ;
#7886 = VECTOR ( 'NONE', #14168, 1000.000000000000000 ) ;
#7887 = ORIENTED_EDGE ( 'NONE', *, *, #21481, .F. ) ;
#7888 = LINE ( 'NONE', #15167, #15201 ) ;
#7889 = DIRECTION ( 'NONE',  ( -0.9874789572432817186, 0.1577507813030449846, 2.556342494820729215E-14 ) ) ;
#7890 = VERTEX_POINT ( 'NONE', #18356 ) ;
#7891 = CARTESIAN_POINT ( 'NONE',  ( -20.55139866881591715, 40.46905695072928211, -146.1780460798107981 ) ) ;
#7892 = ADVANCED_FACE ( 'NONE', ( #12989 ), #20263, .F. ) ;
#7893 = CARTESIAN_POINT ( 'NONE',  ( 8.845083429264123609, 38.45981370960942058, -142.0257885890056002 ) ) ;
#7894 = CARTESIAN_POINT ( 'NONE',  ( 7.081342377746940642, 36.51003594057088009, -146.5072937552426708 ) ) ;
#7895 = CARTESIAN_POINT ( 'NONE',  ( -23.20965953747225541, 36.97759979273073583, -140.7013664825230421 ) ) ;
#7896 = DIRECTION ( 'NONE',  ( -1.000000000000000000, 0.000000000000000000, -2.508689552389999873E-12 ) ) ;
#7897 = ORIENTED_EDGE ( 'NONE', *, *, #10482, .F. ) ;
#7898 = VECTOR ( 'NONE', #852, 1000.000000000000000 ) ;
#7899 = ADVANCED_FACE ( 'NONE', ( #17021 ), #6550, .F. ) ;
#7900 = AXIS2_PLACEMENT_3D ( 'NONE', #2243, #18653, #9467 ) ;
#7901 = EDGE_CURVE ( 'NONE', #21292, #5364, #22618, .T. ) ;
#7902 = FACE_OUTER_BOUND ( 'NONE', #10253, .T. ) ;
#7903 = VECTOR ( 'NONE', #2043, 1000.000000000000114 ) ;
#7904 = ORIENTED_EDGE ( 'NONE', *, *, #14106, .F. ) ;
#7905 = DIRECTION ( 'NONE',  ( -0.9954742291034677226, 0.09503188512734457583, 4.503363594322118746E-12 ) ) ;
#7906 = EDGE_CURVE ( 'NONE', #1168, #11590, #10104, .T. ) ;
#7907 = VERTEX_POINT ( 'NONE', #11535 ) ;
#7908 = ORIENTED_EDGE ( 'NONE', *, *, #14188, .T. ) ;
#7909 = AXIS2_PLACEMENT_3D ( 'NONE', #19624, #3442, #3676 ) ;
#7910 = CARTESIAN_POINT ( 'NONE',  ( -23.12623614695305108, 35.07139013615802270, -139.7131972622368323 ) ) ;
#7911 = EDGE_CURVE ( 'NONE', #5505, #1160, #18812, .T. ) ;
#7912 = ORIENTED_EDGE ( 'NONE', *, *, #13581, .F. ) ;
#7913 = DIRECTION ( 'NONE',  ( 2.257144641401724984E-12, 0.000000000000000000, 1.000000000000000000 ) ) ;
#7914 = ORIENTED_EDGE ( 'NONE', *, *, #19917, .F. ) ;
#7915 = ORIENTED_EDGE ( 'NONE', *, *, #4757, .F. ) ;
#7916 = CARTESIAN_POINT ( 'NONE',  ( -27.87685576917573371, 39.58963625183361046, -147.4493226070128742 ) ) ;
#7917 = DIRECTION ( 'NONE',  ( 0.000000000000000000, 1.000000000000000000, 0.000000000000000000 ) ) ;
#7918 = CARTESIAN_POINT ( 'NONE',  ( 24.89581725840000104, -26.85672394480000236, -144.5552959529999839 ) ) ;
#7919 = FACE_OUTER_BOUND ( 'NONE', #15145, .T. ) ;
#7920 = CARTESIAN_POINT ( 'NONE',  ( -7.104147058966693962, 32.78722980359287220, -146.6177089082302416 ) ) ;
#7921 = VECTOR ( 'NONE', #18019, 1000.000000000000000 ) ;
#7922 = CARTESIAN_POINT ( 'NONE',  ( -8.871724173964516069, 39.55783021574837477, -140.3984215277044711 ) ) ;
#7923 = VERTEX_POINT ( 'NONE', #1093 ) ;
#7924 = DIRECTION ( 'NONE',  ( -2.259525899700000234E-12, 0.000000000000000000, 1.000000000000000000 ) ) ;
#7925 = EDGE_CURVE ( 'NONE', #1756, #7449, #15363, .T. ) ;
#7926 = CARTESIAN_POINT ( 'NONE',  ( 8.500000000060001781, 38.50000000000000000, -146.0552959529999839 ) ) ;
#7927 = CIRCLE ( 'NONE', #2278, 6.999999999999999112 ) ;
#7928 = CARTESIAN_POINT ( 'NONE',  ( -24.63187620858803228, 37.01311550629856839, -148.7335123083400106 ) ) ;
#7929 = ORIENTED_EDGE ( 'NONE', *, *, #9151, .F. ) ;
#7930 = ADVANCED_FACE ( 'NONE', ( #13336 ), #2762, .T. ) ;
#7931 = CARTESIAN_POINT ( 'NONE',  ( -13.11071995283477953, 37.07027326795081734, -147.8134892432882452 ) ) ;
#7932 = EDGE_CURVE ( 'NONE', #1705, #16883, #4767, .T. ) ;
#7933 = CARTESIAN_POINT ( 'NONE',  ( -18.64767072899999789, 38.89869937459999960, -148.1651290810000319 ) ) ;
#7934 = CYLINDRICAL_SURFACE ( 'NONE', #23221, 9.000000000000000000 ) ;
#7935 = ORIENTED_EDGE ( 'NONE', *, *, #15610, .T. ) ;
#7936 = SURFACE_STYLE_USAGE ( .BOTH. , #9832 ) ;
#7937 = CARTESIAN_POINT ( 'NONE',  ( 19.13369214859999801, -51.00000000000000000, -136.0552959530000123 ) ) ;
#7938 = AXIS2_PLACEMENT_3D ( 'NONE', #15733, #22993, #12154 ) ;
#7939 = ORIENTED_EDGE ( 'NONE', *, *, #905, .T. ) ;
#7940 = DIRECTION ( 'NONE',  ( 8.955190032049920155E-12, -9.104778821555109033E-13, 1.000000000000000000 ) ) ;
#7941 = PLANE ( 'NONE',  #19469 ) ;
#7942 = ORIENTED_EDGE ( 'NONE', *, *, #2070, .F. ) ;
#7943 = CARTESIAN_POINT ( 'NONE',  ( -2.499999999949999996, 31.50000000000000000, -150.0552959529999839 ) ) ;
#7944 =( REPRESENTATION_RELATIONSHIP ('NONE','NONE', #7672, #538 ) REPRESENTATION_RELATIONSHIP_WITH_TRANSFORMATION ( #7421 )SHAPE_REPRESENTATION_RELATIONSHIP( ) );
#7945 = AXIS2_PLACEMENT_3D ( 'NONE', #16419, #4034, #129 ) ;
#7946 = CARTESIAN_POINT ( 'NONE',  ( -19.89002371296891880, 39.36161564549420433, -140.9617346337927870 ) ) ;
#7947 = ORIENTED_EDGE ( 'NONE', *, *, #1439, .F. ) ;
#7948 = PLANE ( 'NONE',  #20203 ) ;
#7949 = VECTOR ( 'NONE', #15315, 1000.000000000000000 ) ;
#7950 = DIRECTION ( 'NONE',  ( 4.533528609800090131E-12, 0.000000000000000000, 1.000000000000000000 ) ) ;
#7951 = EDGE_LOOP ( 'NONE', ( #21585, #1442, #6118, #21195 ) ) ;
#7952 = VECTOR ( 'NONE', #19246, 1000.000000000000000 ) ;
#7953 = LINE ( 'NONE', #20469, #7181 ) ;
#7954 = DIRECTION ( 'NONE',  ( 8.955190032050000935E-12, -9.104778821549999739E-13, 1.000000000000000000 ) ) ;
#7955 = FACE_OUTER_BOUND ( 'NONE', #2927, .T. ) ;
#7956 = ORIENTED_EDGE ( 'NONE', *, *, #17430, .F. ) ;
#7957 = DIRECTION ( 'NONE',  ( -2.507771768020000122E-12, -0.000000000000000000, 1.000000000000000000 ) ) ;
#7958 = DIRECTION ( 'NONE',  ( -1.000000000000000000, 0.000000000000000000, 2.257171095940000041E-12 ) ) ;
#7959 = VERTEX_POINT ( 'NONE', #4412 ) ;
#7960 = ORIENTED_EDGE ( 'NONE', *, *, #231, .T. ) ;
#7961 = VECTOR ( 'NONE', #19805, 1000.000000000000227 ) ;
#7962 = CIRCLE ( 'NONE', #15967, 2.000000000000000000 ) ;
#7963 = CARTESIAN_POINT ( 'NONE',  ( 2.656359840075251277, -1.100999472805462398, -150.0552959529999839 ) ) ;
#7964 = ADVANCED_FACE ( 'NONE', ( #7852 ), #739, .T. ) ;
#7965 = CARTESIAN_POINT ( 'NONE',  ( -29.88845675159999971, 40.47687533140000227, -144.8298193859999969 ) ) ;
#7966 = AXIS2_PLACEMENT_3D ( 'NONE', #3665, #19964, #1661 ) ;
#7967 = AXIS2_PLACEMENT_3D ( 'NONE', #8773, #1903, #7003 ) ;
#7968 = ADVANCED_FACE ( 'NONE', ( #8092 ), #18928, .F. ) ;
#7969 = DIRECTION ( 'NONE',  ( 2.257171095940000041E-12, 1.003664318209372040E-28, 1.000000000000000000 ) ) ;
#7970 = CARTESIAN_POINT ( 'NONE',  ( -20.60824191589811605, -4.000000000000000000, -146.3157682190056335 ) ) ;
#7971 = VERTEX_POINT ( 'NONE', #13563 ) ;
#7972 = DIRECTION ( 'NONE',  ( -0.9832226533249337486, 0.1824094679249879947, 1.246536736419916629E-15 ) ) ;
#7973 = PLANE ( 'NONE',  #18829 ) ;
#7974 = CARTESIAN_POINT ( 'NONE',  ( 4.499999999879999102, -3.500000000000000000, -139.0552959529999839 ) ) ;
#7975 = CARTESIAN_POINT ( 'NONE',  ( -8.931798216517609745, 36.92954985152155700, -147.9669232059208070 ) ) ;
#7976 = CARTESIAN_POINT ( 'NONE',  ( -23.34997301937064051, 41.23575095005864455, -144.6233831888736177 ) ) ;
#7977 = CARTESIAN_POINT ( 'NONE',  ( -17.52779041586176945, 36.93962571632794578, -139.7364823516872434 ) ) ;
#7978 = FACE_OUTER_BOUND ( 'NONE', #15437, .T. ) ;
#7979 = DIRECTION ( 'NONE',  ( 1.000000000000000000, 0.000000000000000000, 0.000000000000000000 ) ) ;
#7980 = CARTESIAN_POINT ( 'NONE',  ( -32.50000000000000000, -2.273736754430000208E-12, -136.0552959530000123 ) ) ;
#7981 = VECTOR ( 'NONE', #5941, 1000.000000000000000 ) ;
#7982 = VECTOR ( 'NONE', #19711, 1000.000000000000000 ) ;
#7983 = ORIENTED_EDGE ( 'NONE', *, *, #11097, .F. ) ;
#7984 = CARTESIAN_POINT ( 'NONE',  ( -9.651143958800396661, 32.86909415028417669, -144.2000375143311715 ) ) ;
#7985 = CARTESIAN_POINT ( 'NONE',  ( -7.337311498550000088, -24.10744501490000147, -148.5552959529999839 ) ) ;
#7986 = ORIENTED_EDGE ( 'NONE', *, *, #7901, .F. ) ;
#7987 = FILL_AREA_STYLE_COLOUR ( '', #18286 ) ;
#7988 = CARTESIAN_POINT ( 'NONE',  ( -22.60316433423102822, 33.52336180732346804, -143.6562582910067363 ) ) ;
#7989 = DIRECTION ( 'NONE',  ( 1.000000000000000000, 0.000000000000000000, 0.000000000000000000 ) ) ;
#7990 = ORIENTED_EDGE ( 'NONE', *, *, #22956, .F. ) ;
#7991 = CARTESIAN_POINT ( 'NONE',  ( -12.73635673082345576, 33.27079122909506026, -143.7284791742528114 ) ) ;
#7992 = EDGE_CURVE ( 'NONE', #16708, #20624, #20836, .T. ) ;
#7993 = CARTESIAN_POINT ( 'NONE',  ( -16.55827375309849714, 37.05535324330074332, -139.5705083843459136 ) ) ;
#7994 = CARTESIAN_POINT ( 'NONE',  ( -15.46613156839999981, 36.99333119719999985, -147.5584717940000132 ) ) ;
#7995 = CARTESIAN_POINT ( 'NONE',  ( 19.27350934360000068, -50.38169314270000143, -149.5552959529999839 ) ) ;
#7996 = LINE ( 'NONE', #291, #6358 ) ;
#7997 = ADVANCED_FACE ( 'NONE', ( #9987 ), #17264, .F. ) ;
#7998 = DIRECTION ( 'NONE',  ( 2.257157423930000049E-12, 0.000000000000000000, 1.000000000000000000 ) ) ;
#7999 = MECHANICAL_DESIGN_GEOMETRIC_PRESENTATION_REPRESENTATION (  '', ( #22450 ), #17508 ) ;
#8000 = CARTESIAN_POINT ( 'NONE',  ( -8.292543378966758638, 38.36969968732901037, -140.9136116612680780 ) ) ;
#8001 = ORIENTED_EDGE ( 'NONE', *, *, #14623, .T. ) ;
#8002 = CARTESIAN_POINT ( 'NONE',  ( 7.683200060759999950, -19.50000000000000000, -148.5552959529999839 ) ) ;
#8003 = ORIENTED_EDGE ( 'NONE', *, *, #16525, .T. ) ;
#8004 = CARTESIAN_POINT ( 'NONE',  ( -14.01657753848344079, 36.22806874879579908, -140.5479840251611847 ) ) ;
#8005 = CARTESIAN_POINT ( 'NONE',  ( -29.04405754849999965, 38.20917013909999582, -139.5702141479999909 ) ) ;
#8006 = CARTESIAN_POINT ( 'NONE',  ( 3.999999999879999546, -3.500000000000000000, -135.4552959529999896 ) ) ;
#8007 = EDGE_LOOP ( 'NONE', ( #654, #17705, #9921, #4372 ) ) ;
#8008 = DIRECTION ( 'NONE',  ( -1.000000000000000000, -2.808280234649999694E-18, -2.507771768019999718E-12 ) ) ;
#8009 = LINE ( 'NONE', #20301, #1921 ) ;
#8010 = CLOSED_SHELL ( 'NONE', ( #5908, #13107, #22341, #11317, #3634, #4085, #8503, #5891, #12113, #16102, #20073 ) ) ;
#8011 = VERTEX_POINT ( 'NONE', #11896 ) ;
#8012 = AXIS2_PLACEMENT_3D ( 'NONE', #23506, #20294, #3524 ) ;
#8013 = CARTESIAN_POINT ( 'NONE',  ( -19.89002371286244042, 39.36161564562564052, -140.9617346336366097 ) ) ;
#8014 = CARTESIAN_POINT ( 'NONE',  ( -17.98964812789086309, 38.50830570032488254, -147.4920370692890117 ) ) ;
#8015 = FACE_OUTER_BOUND ( 'NONE', #12087, .T. ) ;
#8016 = CARTESIAN_POINT ( 'NONE',  ( 0.3832000607639999834, -24.50000000000000000, -148.5552959529999839 ) ) ;
#8017 = CARTESIAN_POINT ( 'NONE',  ( -26.07820652087960056, 36.26055466349079381, -140.6390304775231925 ) ) ;
#8018 = EDGE_CURVE ( 'NONE', #18803, #15247, #12070, .T. ) ;
#8019 = EDGE_LOOP ( 'NONE', ( #1592, #13787, #8529, #21823 ) ) ;
#8020 = CARTESIAN_POINT ( 'NONE',  ( 1.133692148550000001, -51.50000000000000000, -134.3952035990000127 ) ) ;
#8021 = ORIENTED_EDGE ( 'NONE', *, *, #8899, .F. ) ;
#8022 = CARTESIAN_POINT ( 'NONE',  ( 32.50000000000000000, -40.03620104880000241, -142.8052959529999839 ) ) ;
#8023 = VECTOR ( 'NONE', #5362, 1000.000000000000000 ) ;
#8024 = VECTOR ( 'NONE', #10488, 1000.000000000000114 ) ;
#8025 = CIRCLE ( 'NONE', #17566, 35.00000000000000000 ) ;
#8027 = ORIENTED_EDGE ( 'NONE', *, *, #14919, .T. ) ;
#8026 = PRODUCT_RELATED_PRODUCT_CATEGORY ( 'part', '', ( #1629 ) ) ;
#8028 = CARTESIAN_POINT ( 'NONE',  ( -30.50000000000000000, 37.00000000000000000, -149.0552959529999839 ) ) ;
#8029 = ORIENTED_EDGE ( 'NONE', *, *, #2127, .F. ) ;
#8030 = CARTESIAN_POINT ( 'NONE',  ( 19.13369214859999801, -50.50000000000000000, -137.0552959530000123 ) ) ;
#8031 = ADVANCED_FACE ( 'NONE', ( #19764 ), #14398, .F. ) ;
#8032 = ORIENTED_EDGE ( 'NONE', *, *, #17674, .F. ) ;
#8033 = PLANE ( 'NONE',  #12916 ) ;
#8034 = ORIENTED_EDGE ( 'NONE', *, *, #13135, .F. ) ;
#8035 = ORIENTED_EDGE ( 'NONE', *, *, #14126, .F. ) ;
#8036 = DIRECTION ( 'NONE',  ( 0.000000000000000000, -1.000000000000000000, 0.000000000000000000 ) ) ;
#8037 = FACE_OUTER_BOUND ( 'NONE', #14841, .T. ) ;
#8038 = CARTESIAN_POINT ( 'NONE',  ( -12.50000000000000000, -2.273736754430000208E-12, -136.0552959530000123 ) ) ;
#8039 =( NAMED_UNIT ( * ) PLANE_ANGLE_UNIT ( ) SI_UNIT ( $, .RADIAN. ) );
#8040 = FACE_OUTER_BOUND ( 'NONE', #15731, .T. ) ;
#8041 = EDGE_CURVE ( 'NONE', #20008, #6667, #12132, .T. ) ;
#8042 = CARTESIAN_POINT ( 'NONE',  ( -9.410006930593050711, 41.20806710879531920, -146.3969463093499712 ) ) ;
#8043 = EDGE_LOOP ( 'NONE', ( #19085, #19849, #20706, #4833 ) ) ;
#8044 = FACE_OUTER_BOUND ( 'NONE', #9451, .T. ) ;
#8045 = VECTOR ( 'NONE', #8889, 1000.000000000000000 ) ;
#8046 = EDGE_CURVE ( 'NONE', #6561, #20464, #5660, .T. ) ;
#8047 = FACE_OUTER_BOUND ( 'NONE', #4723, .T. ) ;
#8048 = DIRECTION ( 'NONE',  ( 0.000000000000000000, 1.000000000000000000, 0.000000000000000000 ) ) ;
#8049 = ORIENTED_EDGE ( 'NONE', *, *, #8382, .T. ) ;
#8050 = FACE_BOUND ( 'NONE', #2749, .T. ) ;
#8051 = CARTESIAN_POINT ( 'NONE',  ( -8.823001505574659120, -11.89636386765829812, -143.5552959529989892 ) ) ;
#8052 = ORIENTED_EDGE ( 'NONE', *, *, #16575, .T. ) ;
#8053 =( NAMED_UNIT ( * ) PLANE_ANGLE_UNIT ( ) SI_UNIT ( $, .RADIAN. ) );
#8054 = FACE_OUTER_BOUND ( 'NONE', #15965, .T. ) ;
#8055 = ORIENTED_EDGE ( 'NONE', *, *, #15697, .F. ) ;
#8056 = CARTESIAN_POINT ( 'NONE',  ( 15.87827223000000032, -26.60524292859999917, -143.5552959529999839 ) ) ;
#8057 = LINE ( 'NONE', #6522, #16032 ) ;
#8058 = VERTEX_POINT ( 'NONE', #19527 ) ;
#8059 = CARTESIAN_POINT ( 'NONE',  ( -14.02405267930000043, 37.94700976039999318, -139.5674429869999926 ) ) ;
#8060 = EDGE_CURVE ( 'NONE', #5378, #19876, #4885, .T. ) ;
#8061 = CARTESIAN_POINT ( 'NONE',  ( -26.41321238348850642, 35.27984194833333476, -140.3745674731081579 ) ) ;
#8062 = EDGE_CURVE ( 'NONE', #3729, #2396, #1573, .T. ) ;
#8063 = PRESENTATION_LAYER_ASSIGNMENT (  '', '', ( #18346 ) ) ;
#8064 = ORIENTED_EDGE ( 'NONE', *, *, #4177, .F. ) ;
#8065 = SURFACE_SIDE_STYLE ('',( #20939 ) ) ;
#8066 = EDGE_CURVE ( 'NONE', #6964, #7124, #14046, .T. ) ;
#8067 = VECTOR ( 'NONE', #17327, 1000.000000000000000 ) ;
#8068 = CARTESIAN_POINT ( 'NONE',  ( -1.000000000000000000, 20.50000000000000000, -150.5552959529999839 ) ) ;
#8069 = EDGE_LOOP ( 'NONE', ( #12876, #6844, #1562, #4126, #16839, #1322, #4381 ) ) ;
#8070 = DIRECTION ( 'NONE',  ( 1.000000000000000000, 0.000000000000000000, 0.000000000000000000 ) ) ;
#8071 = CARTESIAN_POINT ( 'NONE',  ( 22.40884248670000289, -21.39641658300000060, -143.5552959529999839 ) ) ;
#8072 = EDGE_LOOP ( 'NONE', ( #17132, #3589, #3919, #11838 ) ) ;
#8073 = LINE ( 'NONE', #10083, #6826 ) ;
#8074 = ORIENTED_EDGE ( 'NONE', *, *, #10170, .T. ) ;
#8075 = ADVANCED_FACE ( 'NONE', ( #12607 ), #3111, .T. ) ;
#8076 = FACE_OUTER_BOUND ( 'NONE', #23407, .T. ) ;
#8077 = ADVANCED_FACE ( 'NONE', ( #21674 ), #17855, .T. ) ;
#8078 = CARTESIAN_POINT ( 'NONE',  ( -15.75743038489378200, -44.30994315220375057, -136.0552959529644568 ) ) ;
#8079 = ORIENTED_EDGE ( 'NONE', *, *, #22898, .T. ) ;
#8080 = ADVANCED_FACE ( 'NONE', ( #3458 ), #10451, .T. ) ;
#8081 = ADVANCED_BREP_SHAPE_REPRESENTATION ( '', ( #19901, #5025 ), #5779 ) ;
#8082 = EDGE_CURVE ( 'NONE', #13979, #11330, #10568, .T. ) ;
#8083 =( GEOMETRIC_REPRESENTATION_CONTEXT ( 3 ) GLOBAL_UNCERTAINTY_ASSIGNED_CONTEXT ( ( #5640 ) ) GLOBAL_UNIT_ASSIGNED_CONTEXT ( ( #7720, #22246, #22362 ) ) REPRESENTATION_CONTEXT ( 'NONE', 'WORKASPACE' ) );
#8084 = ORIENTED_EDGE ( 'NONE', *, *, #2105, .T. ) ;
#8085 = DIRECTION ( 'NONE',  ( 3.994014902950000436E-29, -1.000000000000000000, 4.148443855749999753E-27 ) ) ;
#8086 = CARTESIAN_POINT ( 'NONE',  ( -30.34130859797645030, 41.26057227206133149, -145.6696127677633967 ) ) ;
#8087 = DIRECTION ( 'NONE',  ( -1.000000000000000000, 0.000000000000000000, 0.000000000000000000 ) ) ;
#8088 = CARTESIAN_POINT ( 'NONE',  ( -20.68907173818941203, -3.608510005926304665, -146.3157682189983007 ) ) ;
#8089 = VERTEX_POINT ( 'NONE', #12480 ) ;
#8090 = CARTESIAN_POINT ( 'NONE',  ( 22.27792782919999937, -15.32580087659999890, -145.5552959529999839 ) ) ;
#8091 = DIRECTION ( 'NONE',  ( 0.000000000000000000, 1.000000000000000000, 0.000000000000000000 ) ) ;
#8092 = FACE_OUTER_BOUND ( 'NONE', #833, .T. ) ;
#8093 = DIRECTION ( 'NONE',  ( -0.9840552701943220404, 0.1778629393740580045, 0.000000000000000000 ) ) ;
#8094 = DIRECTION ( 'NONE',  ( 1.000000000000000000, 0.000000000000000000, 0.000000000000000000 ) ) ;
#8095 = FACE_OUTER_BOUND ( 'NONE', #16995, .T. ) ;
#8096 = CARTESIAN_POINT ( 'NONE',  ( -17.08496771056256947, 36.30549575163614406, -140.6791867003299785 ) ) ;
#8097 = CARTESIAN_POINT ( 'NONE',  ( -21.35824191589999899, -4.000000000000000000, -146.2257682199999920 ) ) ;
#8098 = DIRECTION ( 'NONE',  ( -0.9913873220698726785, 0.1309625047069831461, -1.853446743629759619E-14 ) ) ;
#8099 = CARTESIAN_POINT ( 'NONE',  ( 11.68320006079999906, -20.50000000000000000, -149.3052959529999839 ) ) ;
#8100 = ORIENTED_EDGE ( 'NONE', *, *, #15819, .F. ) ;
#8101 = CARTESIAN_POINT ( 'NONE',  ( -10.27640102954716816, 33.81552902124293780, -145.7376306576129537 ) ) ;
#8102 = DIRECTION ( 'NONE',  ( 1.000000000000000000, 0.000000000000000000, -1.526556658859589738E-13 ) ) ;
#8103 = EDGE_CURVE ( 'NONE', #12665, #19198, #13926, .T. ) ;
#8104 = DIRECTION ( 'NONE',  ( 1.526468026910264955E-13, 8.159623473499449847E-13, 1.000000000000000000 ) ) ;
#8105 = ORIENTED_EDGE ( 'NONE', *, *, #417, .T. ) ;
#8106 = DIRECTION ( 'NONE',  ( -3.994014902950000436E-29, 1.000000000000000000, -4.148443855749999753E-27 ) ) ;
#8107 = FACE_OUTER_BOUND ( 'NONE', #17292, .T. ) ;
#8108 = ORIENTED_EDGE ( 'NONE', *, *, #21890, .F. ) ;
#8109 = CARTESIAN_POINT ( 'NONE',  ( -23.20965953746479116, 36.97759979273159558, -140.7013664825302612 ) ) ;
#8110 = CARTESIAN_POINT ( 'NONE',  ( -5.500000000000000000, 44.50000000000000000, -150.0552959529999839 ) ) ;
#8111 = CARTESIAN_POINT ( 'NONE',  ( 4.084222279812038003, 13.38246373452152227, -150.0552959529999839 ) ) ;
#8112 = DIRECTION ( 'NONE',  ( 0.000000000000000000, 1.000000000000000000, 0.000000000000000000 ) ) ;
#8113 = CARTESIAN_POINT ( 'NONE',  ( -1.000000000000000000, 20.50000000000000000, -150.0552959529999839 ) ) ;
#8114 = CARTESIAN_POINT ( 'NONE',  ( 10.68320006080000084, -20.50000000000000000, -149.3052959529999839 ) ) ;
#8115 = CARTESIAN_POINT ( 'NONE',  ( -7.529689113779999943, 37.05876528330000497, -139.9906690790000141 ) ) ;
#8116 = AXIS2_PLACEMENT_3D ( 'NONE', #14668, #17893, #20033 ) ;
#8117 = ORIENTED_EDGE ( 'NONE', *, *, #684, .F. ) ;
#8118 = CARTESIAN_POINT ( 'NONE',  ( 8.750000000000000000, -38.23606797749999942, -150.5552959529999839 ) ) ;
#8119 = SURFACE_STYLE_USAGE ( .BOTH. , #5990 ) ;
#8120 = VERTEX_POINT ( 'NONE', #21315 ) ;
#8121 = CARTESIAN_POINT ( 'NONE',  ( -14.50908993377715639, 36.94185792197168894, -140.4668331871908435 ) ) ;
#8122 = DIRECTION ( 'NONE',  ( 0.000000000000000000, -1.000000000000000000, 0.000000000000000000 ) ) ;
#8123 = LINE ( 'NONE', #4451, #19139 ) ;
#8124 = ORIENTED_EDGE ( 'NONE', *, *, #4090, .F. ) ;
#8125 = EDGE_CURVE ( 'NONE', #7013, #22055, #10227, .T. ) ;
#8126 = DIRECTION ( 'NONE',  ( 0.000000000000000000, -0.4794255386042052813, -0.8775825618903714265 ) ) ;
#8127 = PLANE ( 'NONE',  #12536 ) ;
#8128 = EDGE_CURVE ( 'NONE', #14773, #9439, #15715, .T. ) ;
#8129 = VERTEX_POINT ( 'NONE', #21198 ) ;
#8130 = CARTESIAN_POINT ( 'NONE',  ( -32.50000000000000000, -50.50000000000000000, -136.0552959530000123 ) ) ;
#8131 = AXIS2_PLACEMENT_3D ( 'NONE', #8456, #6672, #21801 ) ;
#8132 = CARTESIAN_POINT ( 'NONE',  ( -18.38287346733138250, 37.71117569361661737, -147.4170582157152580 ) ) ;
#8133 = PLANE ( 'NONE',  #22404 ) ;
#8134 = DIRECTION ( 'NONE',  ( -5.094701932209999624E-24, -1.000000000000000000, 1.149947916579999802E-35 ) ) ;
#8135 = CARTESIAN_POINT ( 'NONE',  ( -24.36912841293447940, 34.40976477756748153, -147.5507798125887859 ) ) ;
#8136 = FACE_OUTER_BOUND ( 'NONE', #7683, .T. ) ;
#8137 = EDGE_CURVE ( 'NONE', #19198, #17357, #5116, .T. ) ;
#8138 = ORIENTED_EDGE ( 'NONE', *, *, #21600, .T. ) ;
#8139 = DIRECTION ( 'NONE',  ( 1.000000000000000000, -5.094701932209999624E-24, 0.000000000000000000 ) ) ;
#8140 = EDGE_LOOP ( 'NONE', ( #5791, #1782, #11006, #8613 ) ) ;
#8141 = ORIENTED_EDGE ( 'NONE', *, *, #7780, .T. ) ;
#8142 = CARTESIAN_POINT ( 'NONE',  ( 2.500000000170000014, 16.50000000000000000, -136.5552959530000123 ) ) ;
#8143 = ORIENTED_EDGE ( 'NONE', *, *, #16811, .T. ) ;
#8144 = VECTOR ( 'NONE', #4182, 1000.000000000000000 ) ;
#8145 = CARTESIAN_POINT ( 'NONE',  ( 3.611688725869999975E-11, 50.50000000000000000, -136.0552959530000123 ) ) ;
#8146 = ORIENTED_EDGE ( 'NONE', *, *, #8806, .F. ) ;
#8147 = VERTEX_POINT ( 'NONE', #3332 ) ;
#8148 = EDGE_CURVE ( 'NONE', #21739, #11298, #8791, .T. ) ;
#8149 = DIRECTION ( 'NONE',  ( 1.000000000000000000, 2.602084704489999637E-17, 0.000000000000000000 ) ) ;
#8150 = LINE ( 'NONE', #18765, #20134 ) ;
#8151 = CARTESIAN_POINT ( 'NONE',  ( -11.57675713931716821, 40.11775891596531807, -142.3540931478985669 ) ) ;
#8152 = EDGE_CURVE ( 'NONE', #16321, #2789, #22240, .T. ) ;
#8153 = CARTESIAN_POINT ( 'NONE',  ( -12.28014746100000032, 36.97113097969999984, -148.4919582129999753 ) ) ;
#8154 = CARTESIAN_POINT ( 'NONE',  ( -8.060221343263076932, 34.98053230926937118, -139.6932736515213662 ) ) ;
#8155 = CARTESIAN_POINT ( 'NONE',  ( -9.213999483924272482, 36.96323514650488562, -148.5699756000874459 ) ) ;
#8156 = VERTEX_POINT ( 'NONE', #356 ) ;
#8157 = FACE_OUTER_BOUND ( 'NONE', #18300, .T. ) ;
#8158 = CARTESIAN_POINT ( 'NONE',  ( 9.412777748462794136, 38.19458062236940776, -146.2522771197201905 ) ) ;
#8159 = ORIENTED_CLOSED_SHELL ( 'NONE', *, #7271, .F. );
#8160 = VECTOR ( 'NONE', #7313, 999.9999999999998863 ) ;
#8161 = CARTESIAN_POINT ( 'NONE',  ( 1.713198289059999935, -17.44292009260000142, -148.5552959529999839 ) ) ;
#8162 = ORIENTED_EDGE ( 'NONE', *, *, #19273, .T. ) ;
#8163 = CARTESIAN_POINT ( 'NONE',  ( -17.69217738326715761, 38.58884013740755137, -147.7569206260365036 ) ) ;
#8164 = DIRECTION ( 'NONE',  ( 1.211690350419999855E-27, 2.765629237170000203E-27, -1.000000000000000000 ) ) ;
#8165 = ORIENTED_EDGE ( 'NONE', *, *, #6685, .T. ) ;
#8166 = CARTESIAN_POINT ( 'NONE',  ( 29.68320006080000084, -7.750000000000000000, -148.5552959529999839 ) ) ;
#8167 = LINE ( 'NONE', #19497, #15410 ) ;
#8168 = ADVANCED_FACE ( 'NONE', ( #19882 ), #19992, .F. ) ;
#8169 = ORIENTED_EDGE ( 'NONE', *, *, #150, .T. ) ;
#8170 = CARTESIAN_POINT ( 'NONE',  ( -6.072796602490000417, -14.62912504250000012, -143.5552959529999839 ) ) ;
#8171 = FACE_OUTER_BOUND ( 'NONE', #14295, .T. ) ;
#8172 = ORIENTED_EDGE ( 'NONE', *, *, #11550, .T. ) ;
#8173 = DIRECTION ( 'NONE',  ( -1.000000000000000000, 5.094701932209999624E-24, 2.257144641399999941E-12 ) ) ;
#8174 = CARTESIAN_POINT ( 'NONE',  ( -26.61369313923914603, 36.92937183404335855, -140.1328975134355517 ) ) ;
#8175 = ORIENTED_EDGE ( 'NONE', *, *, #15661, .F. ) ;
#8176 =( LENGTH_UNIT ( ) NAMED_UNIT ( * ) SI_UNIT ( .MILLI., .METRE. ) );
#8177 = LINE ( 'NONE', #6180, #19016 ) ;
#8178 = EDGE_LOOP ( 'NONE', ( #3944, #18391, #23174, #3408 ) ) ;
#8179 = LINE ( 'NONE', #10077, #4163 ) ;
#8180 = VECTOR ( 'NONE', #3081, 1000.000000000000000 ) ;
#8181 = DIRECTION ( 'NONE',  ( 1.000000000000000000, 2.004714280773594901E-17, -1.095180403012019938E-17 ) ) ;
#8182 = ORIENTED_EDGE ( 'NONE', *, *, #13587, .F. ) ;
#8183 = EDGE_CURVE ( 'NONE', #2237, #3754, #1907, .T. ) ;
#8184 = VECTOR ( 'NONE', #1735, 1000.000000000000000 ) ;
#8185 = CARTESIAN_POINT ( 'NONE',  ( 16.16922456049999823, -22.27514461170000004, -147.5552959529999839 ) ) ;
#8186 = VERTEX_POINT ( 'NONE', #5817 ) ;
#8187 = DIRECTION ( 'NONE',  ( 1.000000000000000000, 0.000000000000000000, 2.507771768019999718E-12 ) ) ;
#8188 = DIRECTION ( 'NONE',  ( 1.000000000000000000, 0.000000000000000000, 0.000000000000000000 ) ) ;
#8189 = ORIENTED_EDGE ( 'NONE', *, *, #23203, .T. ) ;
#8190 = B_SPLINE_CURVE_WITH_KNOTS ( 'NONE', 5,
 ( #13183, #20456, #14868, #11388, #586, #5697, #11047, #16990, #13071, #15091, #18433, #22353 ),
 .UNSPECIFIED., .F., .F.,
 ( 6, 3, 3, 6 ),
 ( 0.000000000000000000, 4.346865784160000246, 8.778337911509998648, 13.29702284770000098 ),
 .UNSPECIFIED. ) ;
#8191 = ADVANCED_FACE ( 'NONE', ( #478 ), #14980, .T. ) ;
#8192 = ORIENTED_EDGE ( 'NONE', *, *, #20666, .T. ) ;
#8193 = CARTESIAN_POINT ( 'NONE',  ( -31.00000000000000000, 1.000000000000000000, -150.5552959529999839 ) ) ;
#8194 = CARTESIAN_POINT ( 'NONE',  ( -33.50000000000000000, 48.00000000000000000, -141.5552959529999839 ) ) ;
#8195 = CARTESIAN_POINT ( 'NONE',  ( -20.60824191589186327, -32.00000000000000000, -149.4708568729739966 ) ) ;
#8196 = CARTESIAN_POINT ( 'NONE',  ( 1.364575185789999923, -21.31553777220000256, -142.5552959529999839 ) ) ;
#8197 = PRODUCT_DEFINITION_SHAPE ( 'NONE', 'NONE',  #23550 ) ;
#8198 = AXIS2_PLACEMENT_3D ( 'NONE', #7393, #16664, #12979 ) ;
#8199 = EDGE_LOOP ( 'NONE', ( #19667, #19295 ) ) ;
#8200 = DIRECTION ( 'NONE',  ( -2.257242012349999735E-12, 0.000000000000000000, 1.000000000000000000 ) ) ;
#8201 = AXIS2_PLACEMENT_3D ( 'NONE', #5753, #21599, #21948 ) ;
#8202 = CARTESIAN_POINT ( 'NONE',  ( -12.50000000000000000, 0.000000000000000000, -150.0552959529999839 ) ) ;
#8203 = EDGE_CURVE ( 'NONE', #13434, #7451, #2150, .T. ) ;
#8204 = CARTESIAN_POINT ( 'NONE',  ( 26.50000000000000000, -20.50000000000000000, -150.0552959529999839 ) ) ;
#8205 = CARTESIAN_POINT ( 'NONE',  ( -15.91979154561522947, -41.79923503140520324, -150.0552959529999839 ) ) ;
#8206 = FACE_OUTER_BOUND ( 'NONE', #16893, .T. ) ;
#8207 = EDGE_CURVE ( 'NONE', #22041, #8776, #18545, .T. ) ;
#8208 = ORIENTED_EDGE ( 'NONE', *, *, #3416, .T. ) ;
#8209 = CARTESIAN_POINT ( 'NONE',  ( -7.337311498540000088, -24.10744501490000147, -147.5552959529999839 ) ) ;
#8210 = EDGE_CURVE ( 'NONE', #23370, #16366, #7597, .T. ) ;
#8211 = CARTESIAN_POINT ( 'NONE',  ( -9.895958504584086768, -22.78427602437751176, -145.5552959529979660 ) ) ;
#8212 = EDGE_CURVE ( 'NONE', #14758, #9331, #5478, .T. ) ;
#8213 = CARTESIAN_POINT ( 'NONE',  ( -5.096343650251323076, 36.99112588044069838, -140.7242647647827312 ) ) ;
#8214 = DIRECTION ( 'NONE',  ( 0.6459422414661292189, 0.7633862853691524286, 2.257144641400453113E-12 ) ) ;
#8215 = DIRECTION ( 'NONE',  ( 1.000000000000000000, 0.000000000000000000, -2.273736754430000208E-12 ) ) ;
#8216 = ORIENTED_EDGE ( 'NONE', *, *, #22932, .F. ) ;
#8217 = CARTESIAN_POINT ( 'NONE',  ( -10.28060652869188196, 34.62853500593604394, -147.1732277809310006 ) ) ;
#8218 = CARTESIAN_POINT ( 'NONE',  ( 32.50000000000000000, 0.000000000000000000, -150.0552959529999839 ) ) ;
#8219 = AXIS2_PLACEMENT_3D ( 'NONE', #1153, #21372, #10155 ) ;
#8220 = DIRECTION ( 'NONE',  ( 0.6689647316207368855, 1.740702895989316487E-17, -0.7432941462487078210 ) ) ;
#8221 = VERTEX_POINT ( 'NONE', #9020 ) ;
#8222 = CARTESIAN_POINT ( 'NONE',  ( -7.499999999969999109, 22.50000000000000000, -137.0552959530000123 ) ) ;
#8223 = CARTESIAN_POINT ( 'NONE',  ( -4.499999999919999105, 40.00000000000000000, -135.0552959530000123 ) ) ;
#8224 = CARTESIAN_POINT ( 'NONE',  ( -22.10824191590187837, -4.000000000000000000, -144.8157682189905984 ) ) ;
#8225 = ORIENTED_EDGE ( 'NONE', *, *, #19428, .F. ) ;
#8226 = CARTESIAN_POINT ( 'NONE',  ( -23.58570254345633543, 37.71378429759510453, -140.4235127406076913 ) ) ;
#8227 = FACE_OUTER_BOUND ( 'NONE', #12197, .T. ) ;
#8228 = CARTESIAN_POINT ( 'NONE',  ( 0.5375835489636304754, 15.92407921618091393, -150.0552959529999839 ) ) ;
#8229 = DIRECTION ( 'NONE',  ( -1.000000000000000000, 0.000000000000000000, 0.000000000000000000 ) ) ;
#8230 = CARTESIAN_POINT ( 'NONE',  ( -10.67196964177461638, 33.18472025305887030, -146.1142301646851251 ) ) ;
#8231 = CARTESIAN_POINT ( 'NONE',  ( -9.213999483924276035, 36.96323514650488562, -148.5699756000874743 ) ) ;
#8232 = AXIS2_PLACEMENT_3D ( 'NONE', #8576, #21573, #12037 ) ;
#8233 = CARTESIAN_POINT ( 'NONE',  ( -7.794473646117169530, 37.74767836363313478, -140.6506544358082920 ) ) ;
#8234 = VERTEX_POINT ( 'NONE', #12721 ) ;
#8235 = EDGE_CURVE ( 'NONE', #17964, #7834, #2265, .T. ) ;
#8236 = VECTOR ( 'NONE', #12188, 1000.000000000000000 ) ;
#8237 = SURFACE_STYLE_USAGE ( .BOTH. , #12780 ) ;
#8238 = ORIENTED_EDGE ( 'NONE', *, *, #5585, .T. ) ;
#8239 = CARTESIAN_POINT ( 'NONE',  ( -6.833331567582606958, 33.96895959207153481, -145.8669957953534038 ) ) ;
#8240 = CARTESIAN_POINT ( 'NONE',  ( -20.97542662470000252, 40.85881720449999932, -141.8340754020000247 ) ) ;
#8241 = VERTEX_POINT ( 'NONE', #16306 ) ;
#8242 = CARTESIAN_POINT ( 'NONE',  ( 6.750000000030000002, -44.75000000000000000, -137.0552959530000123 ) ) ;
#8243 = CARTESIAN_POINT ( 'NONE',  ( 19.13369214859999801, -51.50000000000000000, -136.0552959530000123 ) ) ;
#8244 = ORIENTED_EDGE ( 'NONE', *, *, #17681, .F. ) ;
#8245 = DIRECTION ( 'NONE',  ( 0.9944529286486341046, -0.1051825684329612265, -4.470295960598355531E-12 ) ) ;
#8246 = AXIS2_PLACEMENT_3D ( 'NONE', #5724, #12981, #5382 ) ;
#8247 = CARTESIAN_POINT ( 'NONE',  ( -18.08788331821740414, 37.73304001162604493, -147.6923967947956271 ) ) ;
#8248 = VECTOR ( 'NONE', #11324, 1000.000000000000000 ) ;
#8249 = DIRECTION ( 'NONE',  ( -0.9846904924346530086, 0.1743118874569384857, 8.976860394976840322E-12 ) ) ;
#8250 = FACE_BOUND ( 'NONE', #22444, .T. ) ;
#8251 = CARTESIAN_POINT ( 'NONE',  ( 23.40529971389999986, -31.60139774330000151, -148.0552959529999839 ) ) ;
#8252 = APPLICATION_CONTEXT ( 'automotive_design' ) ;
#8253 = CARTESIAN_POINT ( 'NONE',  ( -25.04112998497079445, 35.58084596877723982, -147.3751007919723577 ) ) ;
#8254 = DIRECTION ( 'NONE',  ( 1.000000000000000000, 0.000000000000000000, 0.000000000000000000 ) ) ;
#8255 = ADVANCED_FACE ( 'NONE', ( #7260 ), #14527, .T. ) ;
#8256 = ORIENTED_EDGE ( 'NONE', *, *, #23341, .F. ) ;
#8257 = CARTESIAN_POINT ( 'NONE',  ( 6.477506801250000557, -13.91317765220000169, -147.5552959529999839 ) ) ;
#8258 = UNCERTAINTY_MEASURE_WITH_UNIT (LENGTH_MEASURE( 1.000000000000000082E-05 ), #2820, 'distance_accuracy_value', 'NONE');
#8260 = EDGE_LOOP ( 'NONE', ( #18872, #4361, #9756, #17486 ) ) ;
#8259 = CIRCLE ( 'NONE', #5235, 15.00000000000000000 ) ;
#8261 = PRESENTATION_STYLE_ASSIGNMENT (( #9928 ) ) ;
#8262 = EDGE_LOOP ( 'NONE', ( #22481, #5426, #9842, #20423 ) ) ;
#8263 = CARTESIAN_POINT ( 'NONE',  ( 16.61718498210000305, -18.75502267109999721, -143.5552959529999839 ) ) ;
#8264 = AXIS2_PLACEMENT_3D ( 'NONE', #7478, #11271, #18542 ) ;
#8265 = EDGE_LOOP ( 'NONE', ( #18182, #3363, #19871, #14432, #6369, #19598, #19837 ) ) ;
#8266 = CARTESIAN_POINT ( 'NONE',  ( 5.519240656430695502, 27.95201674008767156, -136.0552959530124895 ) ) ;
#8267 = EDGE_LOOP ( 'NONE', ( #16115, #17294, #14040, #9147 ) ) ;
#8268 = VERTEX_POINT ( 'NONE', #10925 ) ;
#8269 = PRODUCT_DEFINITION_SHAPE ( 'NONE', 'NONE',  #4990 ) ;
#8270 = LINE ( 'NONE', #1169, #13665 ) ;
#8271 = DIRECTION ( 'NONE',  ( 2.257242012349999735E-12, 0.000000000000000000, -1.000000000000000000 ) ) ;
#8272 = CARTESIAN_POINT ( 'NONE',  ( -10.41700570847820551, 37.07221587398769458, -140.3414633426675380 ) ) ;
#8273 = CARTESIAN_POINT ( 'NONE',  ( 0.1832000610750000313, -6.500000000000000000, -150.0552959529999839 ) ) ;
#8274 = CARTESIAN_POINT ( 'NONE',  ( -7.806459626923599515, 32.86659014932959622, -143.7778124396562021 ) ) ;
#8275 = CARTESIAN_POINT ( 'NONE',  ( -8.764208581537477727, 41.80648535992416015, -144.5325683263670271 ) ) ;
#8276 = EDGE_LOOP ( 'NONE', ( #4801, #10669, #21986, #11479 ) ) ;
#8277 = CARTESIAN_POINT ( 'NONE',  ( 23.84377886109999878, -30.60602870049999780, -145.5552959529999839 ) ) ;
#8278 = VECTOR ( 'NONE', #6885, 1000.000000000000000 ) ;
#8279 = CARTESIAN_POINT ( 'NONE',  ( 9.990149291296260614, 37.19975720979747535, -146.5492378968540095 ) ) ;
#8280 = CONICAL_SURFACE ( 'NONE', #9787, 1.499999999999999334, 0.9827937232469998730 ) ;
#8281 = LINE ( 'NONE', #11730, #3786 ) ;
#8282 = ORIENTED_EDGE ( 'NONE', *, *, #13526, .F. ) ;
#8283 = EDGE_CURVE ( 'NONE', #22524, #21589, #12524, .T. ) ;
#8284 = DIRECTION ( 'NONE',  ( -2.507771768019999718E-12, -1.592654864209999947E-17, 1.000000000000000000 ) ) ;
#8285 = FACE_OUTER_BOUND ( 'NONE', #8766, .T. ) ;
#8286 = ORIENTED_EDGE ( 'NONE', *, *, #18549, .F. ) ;
#8287 = DIRECTION ( 'NONE',  ( -1.000000000000000000, 0.000000000000000000, 0.000000000000000000 ) ) ;
#8288 = EDGE_CURVE ( 'NONE', #14413, #20358, #6080, .T. ) ;
#8289 = DIRECTION ( 'NONE',  ( 1.000000000000000000, 0.000000000000000000, -2.257453483404485235E-12 ) ) ;
#8290 = VERTEX_POINT ( 'NONE', #9144 ) ;
#8291 = DIRECTION ( 'NONE',  ( -2.257144641399999941E-12, 8.049635416090000264E-35, -1.000000000000000000 ) ) ;
#8292 = CARTESIAN_POINT ( 'NONE',  ( 24.28524365307784905, -23.42191803000494232, -150.0552959529999839 ) ) ;
#8293 = ORIENTED_EDGE ( 'NONE', *, *, #16787, .F. ) ;
#8294 = DIRECTION ( 'NONE',  ( 5.094701932209999624E-24, 1.000000000000000000, 0.000000000000000000 ) ) ;
#8295 = CARTESIAN_POINT ( 'NONE',  ( -25.70171731128227677, 35.06206091446468776, -139.6775904388746312 ) ) ;
#8296 = ORIENTED_EDGE ( 'NONE', *, *, #907, .T. ) ;
#8297 = AXIS2_PLACEMENT_3D ( 'NONE', #11850, #8407, #15680 ) ;
#8298 = CARTESIAN_POINT ( 'NONE',  ( -8.594304764359998572, -10.75357442870000035, -145.5552959529999839 ) ) ;
#8299 = ORIENTED_EDGE ( 'NONE', *, *, #810, .F. ) ;
#8300 = DIRECTION ( 'NONE',  ( 1.000000000000000000, 0.000000000000000000, 0.000000000000000000 ) ) ;
#8301 = AXIS2_PLACEMENT_3D ( 'NONE', #7378, #5232, #23444 ) ;
#8302 = CARTESIAN_POINT ( 'NONE',  ( -9.790691201043280500, -24.06562932247060260, -147.5552959529991313 ) ) ;
#8303 = ORIENTED_EDGE ( 'NONE', *, *, #20794, .F. ) ;
#8304 = DIRECTION ( 'NONE',  ( 0.1435602414469281940, 0.9896415801065048257, -3.836930773098079160E-13 ) ) ;
#8305 = AXIS2_PLACEMENT_3D ( 'NONE', #3119, #10351, #17626 ) ;
#8306 = ORIENTED_EDGE ( 'NONE', *, *, #18711, .T. ) ;
#8307 = VECTOR ( 'NONE', #3346, 1000.000000000000227 ) ;
#8308 = CARTESIAN_POINT ( 'NONE',  ( 13.68320006080000084, -21.50000000000000000, -148.5552959529999839 ) ) ;
#8309 = FACE_OUTER_BOUND ( 'NONE', #8265, .T. ) ;
#8310 = ORIENTED_EDGE ( 'NONE', *, *, #14834, .T. ) ;
#8311 = VERTEX_POINT ( 'NONE', #7376 ) ;
#8312 = DIRECTION ( 'NONE',  ( -1.000000000000000000, 0.000000000000000000, 0.000000000000000000 ) ) ;
#8313 = VECTOR ( 'NONE', #1241, 1000.000000000000000 ) ;
#8314 = DIRECTION ( 'NONE',  ( 0.000000000000000000, -1.000000000000000000, -1.592654864069999939E-17 ) ) ;
#8315 = VECTOR ( 'NONE', #20779, 1000.000000000000000 ) ;
#8316 = CARTESIAN_POINT ( 'NONE',  ( 2.508811538200000246, -14.35090895149999923, -144.5552959529999839 ) ) ;
#8317 = DIRECTION ( 'NONE',  ( 0.9989565318111731651, 0.04567108003750790235, -1.889135246290330374E-13 ) ) ;
#8318 = VERTEX_POINT ( 'NONE', #5703 ) ;
#8319 = CARTESIAN_POINT ( 'NONE',  ( -16.20103055061850839, -42.07987191916137704, -136.0552959529634620 ) ) ;
#8320 = EDGE_CURVE ( 'NONE', #777, #2111, #12958, .T. ) ;
#8321 = DIRECTION ( 'NONE',  ( -2.257144641399999941E-12, 0.000000000000000000, -1.000000000000000000 ) ) ;
#8322 = VECTOR ( 'NONE', #1425, 999.9999999999998863 ) ;
#8323 = CARTESIAN_POINT ( 'NONE',  ( -7.041959465309999722, -26.08051538799999847, -143.5552959529999839 ) ) ;
#8324 = CARTESIAN_POINT ( 'NONE',  ( -13.69030790613426873, -42.24283201952169975, -150.0552959529999839 ) ) ;
#8325 = CARTESIAN_POINT ( 'NONE',  ( -11.65594158655517454, 36.92432879710629123, -140.1042033531252571 ) ) ;
#8326 = VECTOR ( 'NONE', #8347, 1000.000000000000000 ) ;
#8327 = CARTESIAN_POINT ( 'NONE',  ( -33.42928932190000069, 12.52782287920000037, -146.7500980969999773 ) ) ;
#8328 = ORIENTED_EDGE ( 'NONE', *, *, #768, .T. ) ;
#8329 = CARTESIAN_POINT ( 'NONE',  ( -15.82083308688285506, 33.29371180489421533, -143.4209982738438214 ) ) ;
#8330 = CARTESIAN_POINT ( 'NONE',  ( 2.048233066679999936, -63.64014441970000746, -142.5552959529999839 ) ) ;
#8331 = EDGE_CURVE ( 'NONE', #11233, #17345, #134, .T. ) ;
#8332 = DIRECTION ( 'NONE',  ( -1.000000000000000000, 0.000000000000000000, 2.255973186040000320E-12 ) ) ;
#8333 = FACE_OUTER_BOUND ( 'NONE', #16591, .T. ) ;
#8334 = LINE ( 'NONE', #3229, #17269 ) ;
#8335 = AXIS2_PLACEMENT_3D ( 'NONE', #14246, #5082, #6983 ) ;
#8336 = ORIENTED_EDGE ( 'NONE', *, *, #15129, .T. ) ;
#8337 = CARTESIAN_POINT ( 'NONE',  ( 4.499999999879999102, -4.000000000000000000, -132.3031539049999878 ) ) ;
#8338 = FACE_OUTER_BOUND ( 'NONE', #22776, .T. ) ;
#8339 = FACE_OUTER_BOUND ( 'NONE', #8502, .T. ) ;
#8340 = ORIENTED_EDGE ( 'NONE', *, *, #15670, .F. ) ;
#8341 = AXIS2_PLACEMENT_3D ( 'NONE', #4020, #9464, #13280 ) ;
#8342 = DIRECTION ( 'NONE',  ( 1.000000000000000000, 0.000000000000000000, 0.000000000000000000 ) ) ;
#8343 = AXIS2_PLACEMENT_3D ( 'NONE', #11934, #6352, #23016 ) ;
#8344 = EDGE_CURVE ( 'NONE', #15836, #4200, #5587, .T. ) ;
#8345 = AXIS2_PLACEMENT_3D ( 'NONE', #955, #22714, #13672 ) ;
#8346 = EDGE_CURVE ( 'NONE', #17007, #22008, #6824, .T. ) ;
#8347 = DIRECTION ( 'NONE',  ( 2.256861364460000137E-12, 0.000000000000000000, 1.000000000000000000 ) ) ;
#8348 = LINE ( 'NONE', #17517, #12122 ) ;
#8349 = EDGE_LOOP ( 'NONE', ( #18634, #20792, #19675, #6876 ) ) ;
#8350 = CARTESIAN_POINT ( 'NONE',  ( -23.08033233722681032, 39.09424655247641311, -141.2811153005157507 ) ) ;
#8351 = EDGE_CURVE ( 'NONE', #213, #4867, #2838, .T. ) ;
#8352 = CARTESIAN_POINT ( 'NONE',  ( 23.00000000000000000, 19.50000000000000000, -151.0552959529999839 ) ) ;
#8353 = EDGE_CURVE ( 'NONE', #19783, #22942, #20575, .T. ) ;
#8354 = CARTESIAN_POINT ( 'NONE',  ( 1.799591341878497452, -16.33655707908583565, -144.5552959529918553 ) ) ;
#8355 = DIRECTION ( 'NONE',  ( 0.1435602414469281940, 0.9896415801065048257, -3.836930773098079160E-13 ) ) ;
#8356 = DIRECTION ( 'NONE',  ( 2.257157423930000049E-12, 0.000000000000000000, 1.000000000000000000 ) ) ;
#8357 = FACE_BOUND ( 'NONE', #5590, .T. ) ;
#8358 = CARTESIAN_POINT ( 'NONE',  ( 4.798892695402127373, -33.70134726954550075, -150.0552959529999555 ) ) ;
#8359 = ORIENTED_EDGE ( 'NONE', *, *, #4204, .T. ) ;
#8360 = CIRCLE ( 'NONE', #20916, 2.500000000000000444 ) ;
#8361 = CIRCLE ( 'NONE', #20156, 2.000000000000000888 ) ;
#8362 = DIRECTION ( 'NONE',  ( 1.000000000000000000, 0.000000000000000000, -2.257453483404482811E-12 ) ) ;
#8363 = VECTOR ( 'NONE', #407, 1000.000000000000000 ) ;
#8364 = EDGE_CURVE ( 'NONE', #8849, #8147, #6169, .T. ) ;
#8365 = ORIENTED_EDGE ( 'NONE', *, *, #4998, .T. ) ;
#8366 = CARTESIAN_POINT ( 'NONE',  ( -7.643000129979401258, 33.91462222170895302, -142.3752337145176625 ) ) ;
#8367 = DIRECTION ( 'NONE',  ( 2.256988247090000272E-12, 0.000000000000000000, 1.000000000000000000 ) ) ;
#8368 = CYLINDRICAL_SURFACE ( 'NONE', #6242, 1.500000000000001110 ) ;
#8369 = EDGE_CURVE ( 'NONE', #6817, #18344, #19019, .T. ) ;
#8370 = ORIENTED_EDGE ( 'NONE', *, *, #23141, .F. ) ;
#8371 = DIRECTION ( 'NONE',  ( -2.257144641399999941E-12, 0.000000000000000000, -1.000000000000000000 ) ) ;
#8372 = CARTESIAN_POINT ( 'NONE',  ( -6.615063969075902328, -20.14048105937242283, -145.5552959529732391 ) ) ;
#8373 = VERTEX_POINT ( 'NONE', #8170 ) ;
#8374 = DIRECTION ( 'NONE',  ( 1.000000000000000000, 2.602084704489999637E-17, -2.257171095940000041E-12 ) ) ;
#8375 = EDGE_CURVE ( 'NONE', #11748, #21536, #18674, .T. ) ;
#8376 = CARTESIAN_POINT ( 'NONE',  ( -17.45880800003273592, 39.00787884620090296, -141.2058029617074624 ) ) ;
#8377 = EDGE_CURVE ( 'NONE', #21090, #17829, #15951, .T. ) ;
#8378 = CARTESIAN_POINT ( 'NONE',  ( -18.00000000000001066, -42.60730091830129140, -150.0552959529999839 ) ) ;
#8379 = AXIS2_PLACEMENT_3D ( 'NONE', #17000, #7605, #5593 ) ;
#8380 = CARTESIAN_POINT ( 'NONE',  ( 7.099236174640187969, 36.46126239971106031, -146.4970002627034091 ) ) ;
#8381 = AXIS2_PLACEMENT_3D ( 'NONE', #3377, #16232, #12295 ) ;
#8382 = EDGE_CURVE ( 'NONE', #21201, #2271, #22703, .T. ) ;
#8383 = B_SPLINE_CURVE_WITH_KNOTS ( 'NONE', 3,
 ( #12347, #9250, #3320, #14267, #5218, #20560, #4369, #11494, #693, #16748 ),
 .UNSPECIFIED., .F., .F.,
 ( 4, 2, 2, 2, 4 ),
 ( 0.000000000000000000, 0.2499999999999999445, 0.4999999999999998890, 0.7499999999999998890, 1.000000000000000000 ),
 .UNSPECIFIED. ) ;
#8384 = LINE ( 'NONE', #13861, #22638 ) ;
#8385 = CARTESIAN_POINT ( 'NONE',  ( -25.33725402877131927, 34.39035690824012192, -140.4300890441823810 ) ) ;
#8386 = CARTESIAN_POINT ( 'NONE',  ( -34.50000000000000000, -1.000000000000000000, -151.0552959529999839 ) ) ;
#8387 = PRODUCT_DEFINITION_SHAPE ( 'NONE', 'NONE',  #23543 ) ;
#8388 = CARTESIAN_POINT ( 'NONE',  ( -12.04808041649379824, 40.71874701590343903, -143.7411651110283799 ) ) ;
#8389 = ORIENTED_EDGE ( 'NONE', *, *, #6960, .F. ) ;
#8390 = CARTESIAN_POINT ( 'NONE',  ( -30.49999999990000177, 26.50000000000000000, -147.5552959529999839 ) ) ;
#8391 = VERTEX_POINT ( 'NONE', #17228 ) ;
#8392 = ORIENTED_EDGE ( 'NONE', *, *, #4482, .T. ) ;
#8393 = DIRECTION ( 'NONE',  ( 2.839308199620000013E-14, 3.568879590630000244E-13, 1.000000000000000000 ) ) ;
#8394 = VERTEX_POINT ( 'NONE', #942 ) ;
#8395 = LINE ( 'NONE', #22567, #775 ) ;
#8396 = CARTESIAN_POINT ( 'NONE',  ( -28.42251996826504623, 36.15178013674928792, -139.6484962583844833 ) ) ;
#8397 = ORIENTED_EDGE ( 'NONE', *, *, #12222, .T. ) ;
#8398 = ORIENTED_EDGE ( 'NONE', *, *, #1957, .T. ) ;
#8399 = PLANE ( 'NONE',  #14814 ) ;
#8400 = CARTESIAN_POINT ( 'NONE',  ( -18.85469010170000459, 37.03971195569999963, -148.4264296979999926 ) ) ;
#8401 = PLANE ( 'NONE',  #5781 ) ;
#8402 = LINE ( 'NONE', #15895, #23006 ) ;
#8403 = CARTESIAN_POINT ( 'NONE',  ( -8.309953467205138722, 35.25464643893679551, -140.3668538354673956 ) ) ;
#8404 = EDGE_CURVE ( 'NONE', #14970, #23117, #589, .T. ) ;
#8405 = CARTESIAN_POINT ( 'NONE',  ( -9.834107546974056646, 39.61220777223162770, -147.4819523409258295 ) ) ;
#8406 = ORIENTED_EDGE ( 'NONE', *, *, #8369, .F. ) ;
#8407 = DIRECTION ( 'NONE',  ( 4.510774274160000731E-12, -1.321907670990000086E-13, 1.000000000000000000 ) ) ;
#8408 = EDGE_CURVE ( 'NONE', #16967, #2111, #4154, .T. ) ;
#8409 = CARTESIAN_POINT ( 'NONE',  ( 4.696349540859360516, -5.000000000000000000, -136.0552959530004387 ) ) ;
#8410 = CARTESIAN_POINT ( 'NONE',  ( 22.50000000000000000, 39.50000000000000000, -150.0552959529999839 ) ) ;
#8411 = VECTOR ( 'NONE', #15183, 1000.000000000000000 ) ;
#8412 = ORIENTED_EDGE ( 'NONE', *, *, #7703, .F. ) ;
#8413 = VECTOR ( 'NONE', #7022, 1000.000000000000000 ) ;
#8414 = CARTESIAN_POINT ( 'NONE',  ( 13.13369214870000157, -50.50000000000000000, -136.5552959530000123 ) ) ;
#8415 = FACE_OUTER_BOUND ( 'NONE', #3447, .T. ) ;
#8416 = ORIENTED_EDGE ( 'NONE', *, *, #10004, .T. ) ;
#8417 = FILL_AREA_STYLE ('',( #10065 ) ) ;
#8418 = CARTESIAN_POINT ( 'NONE',  ( 22.50000000000000000, 39.50000000000000000, -151.0552959529999839 ) ) ;
#8419 = EDGE_LOOP ( 'NONE', ( #22245, #71, #12327, #13243 ) ) ;
#8420 = CARTESIAN_POINT ( 'NONE',  ( 32.50000000000000000, 20.96379895120000114, -136.5552959530000123 ) ) ;
#8421 = DIRECTION ( 'NONE',  ( 0.000000000000000000, -1.000000000000000000, 2.257144641399999941E-12 ) ) ;
#8422 = EDGE_LOOP ( 'NONE', ( #16027, #2102, #17525, #14856 ) ) ;
#8423 = CARTESIAN_POINT ( 'NONE',  ( -15.00096184705712510, 39.32882771142540435, -140.7014506208544731 ) ) ;
#8424 = CARTESIAN_POINT ( 'NONE',  ( -24.53581133586112273, 34.20578514941706771, -147.8660713000161877 ) ) ;
#8425 = ORIENTED_EDGE ( 'NONE', *, *, #3565, .T. ) ;
#8426 = ORIENTED_EDGE ( 'NONE', *, *, #10231, .F. ) ;
#8427 = DIRECTION ( 'NONE',  ( 0.000000000000000000, 0.8775825618903703162, 0.4794255386042076128 ) ) ;
#8428 = PLANE ( 'NONE',  #19472 ) ;
#8429 = VERTEX_POINT ( 'NONE', #20459 ) ;
#8430 = COLOUR_RGB ( '', 0.40784314, 0.44705882, 0.49803922) ;
#8431 = DIRECTION ( 'NONE',  ( 0.7633862853691523176, 0.6459422414661291079, 0.000000000000000000 ) ) ;
#8432 = CIRCLE ( 'NONE', #13754, 7.499999999999999112 ) ;
#8433 = EDGE_CURVE ( 'NONE', #4660, #11114, #20848, .T. ) ;
#8434 = EDGE_CURVE ( 'NONE', #8186, #16725, #4552, .T. ) ;
#8435 = CARTESIAN_POINT ( 'NONE',  ( -35.47299999999999898, 11.04196010839999964, -143.5552959529999839 ) ) ;
#8436 = CARTESIAN_POINT ( 'NONE',  ( 23.50000000000000000, -20.50000000000000000, -135.0552959530000123 ) ) ;
#8437 = ADVANCED_FACE ( 'NONE', ( #15094, #20933, #11867 ), #13306, .T. ) ;
#8438 = ORIENTED_EDGE ( 'NONE', *, *, #15819, .T. ) ;
#8439 = CARTESIAN_POINT ( 'NONE',  ( 24.68320006080000084, -16.50000000000000000, -148.5552959529999839 ) ) ;
#8440 = FACE_OUTER_BOUND ( 'NONE', #702, .T. ) ;
#8441 = CARTESIAN_POINT ( 'NONE',  ( -15.37212823710000009, 38.89807584180000077, -148.3010324070000081 ) ) ;
#8442 = CARTESIAN_POINT ( 'NONE',  ( 10.50000000020000002, 24.50000000000000000, -136.5552959530000123 ) ) ;
#8443 = ORIENTED_EDGE ( 'NONE', *, *, #18529, .T. ) ;
#8444 =( GEOMETRIC_REPRESENTATION_CONTEXT ( 3 ) GLOBAL_UNCERTAINTY_ASSIGNED_CONTEXT ( ( #19693 ) ) GLOBAL_UNIT_ASSIGNED_CONTEXT ( ( #14228, #19474, #6963 ) ) REPRESENTATION_CONTEXT ( 'NONE', 'WORKASPACE' ) );
#8445 = DIRECTION ( 'NONE',  ( 2.257144641399999941E-12, 0.000000000000000000, 1.000000000000000000 ) ) ;
#8446 = AXIS2_PLACEMENT_3D ( 'NONE', #23308, #14506, #7118 ) ;
#8447 = DIRECTION ( 'NONE',  ( 2.259525899719999991E-12, 0.000000000000000000, 1.000000000000000000 ) ) ;
#8448 = DIRECTION ( 'NONE',  ( -1.000000000000000000, 0.000000000000000000, 0.000000000000000000 ) ) ;
#8449 = DIRECTION ( 'NONE',  ( -0.9847555042252370550, 0.1739442350240419932, 7.303835699471759765E-15 ) ) ;
#8450 = CARTESIAN_POINT ( 'NONE',  ( 32.00000000000000000, -40.03620104880000241, -136.0552959530000123 ) ) ;
#8451 = ORIENTED_EDGE ( 'NONE', *, *, #4430, .F. ) ;
#8452 = CARTESIAN_POINT ( 'NONE',  ( -17.03115501030000090, 35.19590004879999867, -139.8299307730000010 ) ) ;
#8453 = CARTESIAN_POINT ( 'NONE',  ( -15.50000000000000000, 47.50000000000000000, -150.0552959529999839 ) ) ;
#8454 = CARTESIAN_POINT ( 'NONE',  ( 2.139623390130000136, -12.81320239329999922, -144.5552959529999839 ) ) ;
#8455 = CARTESIAN_POINT ( 'NONE',  ( -4.855180678435623953, 37.01991258974685906, -139.3889649350432194 ) ) ;
#8456 = CARTESIAN_POINT ( 'NONE',  ( -31.75000000000000000, 19.50000000000000000, -151.0552959529999839 ) ) ;
#8457 = ORIENTED_EDGE ( 'NONE', *, *, #12811, .T. ) ;
#8458 = DIRECTION ( 'NONE',  ( -0.000000000000000000, 1.000000000000000000, 0.000000000000000000 ) ) ;
#8459 = DIRECTION ( 'NONE',  ( 1.000000000000000000, 0.000000000000000000, -2.257120985840000117E-12 ) ) ;
#8460 = CARTESIAN_POINT ( 'NONE',  ( 3.038109793998242214, -3.109613115927613247, -150.0552959530000123 ) ) ;
#8461 = PRESENTATION_LAYER_ASSIGNMENT (  '', '', ( #13037 ) ) ;
#8462 = ADVANCED_FACE ( 'NONE', ( #19136 ), #11506, .T. ) ;
#8463 = ORIENTED_EDGE ( 'NONE', *, *, #5488, .T. ) ;
#8464 = CARTESIAN_POINT ( 'NONE',  ( -28.40010805446878095, 32.24922851640265975, -144.5145871741030135 ) ) ;
#8465 = FACE_OUTER_BOUND ( 'NONE', #22472, .T. ) ;
#8466 = ORIENTED_EDGE ( 'NONE', *, *, #19265, .T. ) ;
#8467 = CARTESIAN_POINT ( 'NONE',  ( -24.13442235245820555, 40.66074140249224200, -143.6722919103460185 ) ) ;
#8468 = DIRECTION ( 'NONE',  ( 0.7071067811865476838, -0.7071067811865475727, 0.000000000000000000 ) ) ;
#8469 = EDGE_CURVE ( 'NONE', #8753, #19783, #22475, .T. ) ;
#8470 = CARTESIAN_POINT ( 'NONE',  ( 2.218297500559999857, -15.44723318490000175, -146.5552959529999839 ) ) ;
#8471 = CARTESIAN_POINT ( 'NONE',  ( 8.225765722546752201, 38.47477381467845703, -142.0366557234719096 ) ) ;
#8472 = EDGE_LOOP ( 'NONE', ( #23246, #4492, #6571, #22154 ) ) ;
#8473 = CARTESIAN_POINT ( 'NONE',  ( -9.213999483942407309, 36.96323514650706699, -148.5699756001263552 ) ) ;
#8474 = CARTESIAN_POINT ( 'NONE',  ( -5.500000000000000000, 44.50000000000000000, -150.5552959529999839 ) ) ;
#8475 = CARTESIAN_POINT ( 'NONE',  ( -7.486908230310626244, 37.06387187510053849, -140.3212062627006560 ) ) ;
#8476 = CARTESIAN_POINT ( 'NONE',  ( 19.27350934360000068, 50.38169314270000143, -150.0552959529999839 ) ) ;
#8477 = VERTEX_POINT ( 'NONE', #18895 ) ;
#8478 = FACE_OUTER_BOUND ( 'NONE', #16128, .T. ) ;
#8479 =( LENGTH_UNIT ( ) NAMED_UNIT ( * ) SI_UNIT ( .MILLI., .METRE. ) );
#8480 = ADVANCED_FACE ( 'NONE', ( #17116 ), #834, .T. ) ;
#8481 = ORIENTED_EDGE ( 'NONE', *, *, #15619, .T. ) ;
#8482 = CARTESIAN_POINT ( 'NONE',  ( -8.411849887981940554, 36.09637009078448244, -140.1322081661286063 ) ) ;
#8483 = DIRECTION ( 'NONE',  ( 0.000000000000000000, 0.000000000000000000, -1.000000000000000000 ) ) ;
#8484 = DIRECTION ( 'NONE',  ( 1.000000000000000000, 0.000000000000000000, 2.504935852220000146E-12 ) ) ;
#8485 = ORIENTED_EDGE ( 'NONE', *, *, #12807, .F. ) ;
#8486 = LINE ( 'NONE', #2796, #2311 ) ;
#8487 = DIRECTION ( 'NONE',  ( -1.000000000000000000, -3.994014902950000436E-29, 0.000000000000000000 ) ) ;
#8488 = EDGE_CURVE ( 'NONE', #7449, #4637, #4498, .T. ) ;
#8489 = ORIENTED_EDGE ( 'NONE', *, *, #4333, .F. ) ;
#8490 = CARTESIAN_POINT ( 'NONE',  ( -22.00705883600000234, 37.05789963359999462, -148.1619053240000028 ) ) ;
#8491 = CARTESIAN_POINT ( 'NONE',  ( -18.09080689940000397, 41.54765954780000214, -144.4256796519999853 ) ) ;
#8492 = CARTESIAN_POINT ( 'NONE',  ( -17.92191803000495298, -42.21475634692217938, -150.0552959530000123 ) ) ;
#8493 = CARTESIAN_POINT ( 'NONE',  ( 6.485119744368450512, -46.75006725843203981, -136.0552959530146211 ) ) ;
#8494 = CARTESIAN_POINT ( 'NONE',  ( -6.389646268321175882, 36.98420143700544571, -147.3954793911336765 ) ) ;
#8495 = ADVANCED_FACE ( 'NONE', ( #17703 ), #12101, .F. ) ;
#8496 = LINE ( 'NONE', #18142, #15085 ) ;
#8497 = DIRECTION ( 'NONE',  ( 1.000000000000000000, 0.000000000000000000, 0.000000000000000000 ) ) ;
#8498 = PLANE ( 'NONE',  #15056 ) ;
#8499 = VERTEX_POINT ( 'NONE', #10425 ) ;
#8500 = CARTESIAN_POINT ( 'NONE',  ( 32.50000000000000000, -39.92025131100000124, -149.5552959529999839 ) ) ;
#8501 = PRODUCT_DEFINITION_CONTEXT ( 'detailed design', #22556, 'design' ) ;
#8502 = EDGE_LOOP ( 'NONE', ( #5598, #19768, #20901, #105 ) ) ;
#8503 = ADVANCED_FACE ( 'NONE', ( #6521 ), #4976, .T. ) ;
#8504 = EDGE_CURVE ( 'NONE', #12619, #10397, #3109, .T. ) ;
#8505 = VERTEX_POINT ( 'NONE', #5089 ) ;
#8506 = DIRECTION ( 'NONE',  ( -1.457881434619999915E-12, 1.723066134219999902E-12, 1.000000000000000000 ) ) ;
#8507 = CARTESIAN_POINT ( 'NONE',  ( -28.50747929780000334, 33.37084171139999711, -143.6371486329999811 ) ) ;
#8508 = ORIENTED_EDGE ( 'NONE', *, *, #17066, .F. ) ;
#8509 = EDGE_CURVE ( 'NONE', #21875, #18822, #21168, .T. ) ;
#8510 = VERTEX_POINT ( 'NONE', #8527 ) ;
#8511 = VECTOR ( 'NONE', #6117, 999.9999999999998863 ) ;
#8512 = CARTESIAN_POINT ( 'NONE',  ( -30.49999999990000177, 29.00000000000000000, -140.5552959529999839 ) ) ;
#8513 = EDGE_CURVE ( 'NONE', #8868, #19550, #23287, .T. ) ;
#8514 = CARTESIAN_POINT ( 'NONE',  ( -19.59255166829999695, 37.05126161860000167, -140.3061871179999969 ) ) ;
#8515 = DIRECTION ( 'NONE',  ( 2.507554887169999917E-12, 0.000000000000000000, -1.000000000000000000 ) ) ;
#8516 = DIRECTION ( 'NONE',  ( 0.000000000000000000, 1.000000000000000000, 0.000000000000000000 ) ) ;
#8517 = VERTEX_POINT ( 'NONE', #17593 ) ;
#8518 = DIRECTION ( 'NONE',  ( 8.955190032050000935E-12, -9.104778821549999739E-13, 1.000000000000000000 ) ) ;
#8519 = CARTESIAN_POINT ( 'NONE',  ( -7.695630400395970128, 37.03895750127041708, -140.6427397355593030 ) ) ;
#8520 = CARTESIAN_POINT ( 'NONE',  ( 25.50006728695417024, 36.10251055749550630, -150.0552959529999839 ) ) ;
#8521 = ORIENTED_EDGE ( 'NONE', *, *, #1533, .F. ) ;
#8522 = CARTESIAN_POINT ( 'NONE',  ( 8.500000000070000894, 37.00000000000000000, -138.5552959529999839 ) ) ;
#8523 = ORIENTED_EDGE ( 'NONE', *, *, #16973, .T. ) ;
#8524 = CARTESIAN_POINT ( 'NONE',  ( 24.85988213910000155, -26.16224997189999968, -145.0552959529999839 ) ) ;
#8525 = CARTESIAN_POINT ( 'NONE',  ( 31.00000000000000000, -0.7500000000009999779, -149.5552959529999839 ) ) ;
#8526 = ORIENTED_EDGE ( 'NONE', *, *, #608, .T. ) ;
#8527 = CARTESIAN_POINT ( 'NONE',  ( -31.00000000000000000, -36.00000000000000000, -150.0552959529999839 ) ) ;
#8528 = DIRECTION ( 'NONE',  ( -1.000000000000000000, 0.000000000000000000, 0.000000000000000000 ) ) ;
#8529 = ORIENTED_EDGE ( 'NONE', *, *, #16678, .T. ) ;
#8530 = CARTESIAN_POINT ( 'NONE',  ( 3.999999999879999546, -4.000000000000000000, -135.0552959530000123 ) ) ;
#8531 = ADVANCED_FACE ( 'NONE', ( #1192 ), #8638, .T. ) ;
#8532 = CARTESIAN_POINT ( 'NONE',  ( -25.54181139845054460, 32.21533750178601707, -143.6018648084610447 ) ) ;
#8533 = VERTEX_POINT ( 'NONE', #23064 ) ;
#8534 =( NAMED_UNIT ( * ) PLANE_ANGLE_UNIT ( ) SI_UNIT ( $, .RADIAN. ) );
#8535 = EDGE_LOOP ( 'NONE', ( #13070, #685, #2328, #19965 ) ) ;
#8536 = CARTESIAN_POINT ( 'NONE',  ( -21.35824191589811605, -3.250000000000000000, -146.3157682190075093 ) ) ;
#8537 = LINE ( 'NONE', #13545, #13778 ) ;
#8538 = ORIENTED_EDGE ( 'NONE', *, *, #14270, .T. ) ;
#8539 = LINE ( 'NONE', #9853, #9083 ) ;
#8540 = FACE_OUTER_BOUND ( 'NONE', #4507, .T. ) ;
#8541 = CARTESIAN_POINT ( 'NONE',  ( -25.33725402870000210, 34.39035690829999936, -140.4300890439999705 ) ) ;
#8542 = VECTOR ( 'NONE', #126, 1000.000000000000000 ) ;
#8543 = ORIENTED_EDGE ( 'NONE', *, *, #4400, .F. ) ;
#8544 = CARTESIAN_POINT ( 'NONE',  ( 8.750000000000000000, -40.23606797749999942, -151.0552959529999839 ) ) ;
#8545 = DIRECTION ( 'NONE',  ( 0.000000000000000000, 1.000000000000000000, 0.000000000000000000 ) ) ;
#8546 = CARTESIAN_POINT ( 'NONE',  ( -15.57786843150000067, 37.00666880280000726, -148.5521201120000114 ) ) ;
#8547 = CARTESIAN_POINT ( 'NONE',  ( -5.070907855429999778, -22.41528233759999722, -147.5552959529999839 ) ) ;
#8548 = ORIENTED_EDGE ( 'NONE', *, *, #4869, .F. ) ;
#8549 = CARTESIAN_POINT ( 'NONE',  ( 10.68320006080000084, -20.50000000000000000, -150.0552959529999839 ) ) ;
#8550 = CARTESIAN_POINT ( 'NONE',  ( -31.99999999949999818, 19.50000000000000000, -137.0552959530000123 ) ) ;
#8551 = DIRECTION ( 'NONE',  ( 1.000000000000000000, 0.000000000000000000, -2.256131789327550371E-12 ) ) ;
#8552 = CARTESIAN_POINT ( 'NONE',  ( -30.49999999990000177, 27.75000000000000000, -147.5552959529999839 ) ) ;
#8553 = DIRECTION ( 'NONE',  ( 2.252420472359999842E-12, 0.000000000000000000, -1.000000000000000000 ) ) ;
#8554 = EDGE_CURVE ( 'NONE', #16332, #10697, #15801, .T. ) ;
#8555 = CARTESIAN_POINT ( 'NONE',  ( -3.499999999969999998, 44.50000000000000000, -137.0552959530000123 ) ) ;
#8556 = AXIS2_PLACEMENT_3D ( 'NONE', #16795, #22616, #2760 ) ;
#8557 = VECTOR ( 'NONE', #16385, 1000.000000000000000 ) ;
#8558 = EDGE_LOOP ( 'NONE', ( #19732, #21493, #15774, #2235 ) ) ;
#8559 = CARTESIAN_POINT ( 'NONE',  ( -16.40179927705826302, 32.92604696800222541, -141.4709451251691235 ) ) ;
#8560 = DIRECTION ( 'NONE',  ( -1.000000000000000000, 5.094701932209999624E-24, 0.000000000000000000 ) ) ;
#8561 = DIRECTION ( 'NONE',  ( -0.7071067811866730279, -0.6205445805637129775, -0.3390050494208429743 ) ) ;
#8562 = DIRECTION ( 'NONE',  ( -2.507771768019999718E-12, -1.592654864069999939E-17, 1.000000000000000000 ) ) ;
#8563 = CARTESIAN_POINT ( 'NONE',  ( 17.06104532839999877, -32.02344838739999489, -143.5552959529999839 ) ) ;
#8564 = ORIENTED_EDGE ( 'NONE', *, *, #13707, .F. ) ;
#8565 = CARTESIAN_POINT ( 'NONE',  ( 21.44117969379999877, -21.36894679869999791, -147.0552959529999839 ) ) ;
#8566 = CARTESIAN_POINT ( 'NONE',  ( 4.499999999879999102, -1.500000000000000000, -135.4552959529999896 ) ) ;
#8567 = ORIENTED_EDGE ( 'NONE', *, *, #6850, .T. ) ;
#8568 =( BOUNDED_CURVE ( )  B_SPLINE_CURVE ( 5, ( #9883, #2773, #876, #11547, #22399, #85 ),
 .UNSPECIFIED., .F., .F. ) 
 B_SPLINE_CURVE_WITH_KNOTS ( ( 6, 6 ),
 ( 1.570796326823717504, 3.141592653590000062 ),
 .UNSPECIFIED. ) 
 CURVE ( )  GEOMETRIC_REPRESENTATION_ITEM ( )  RATIONAL_B_SPLINE_CURVE ( ( 0.2500000000000000000, 0.2500000000036564085, 0.3000000000054846572, 0.4000000000073128392, 0.6000000000073127948, 1.000000000000000000 ) ) 
 REPRESENTATION_ITEM ( '' )  );
#8570 = CARTESIAN_POINT ( 'NONE',  ( -28.98364196379448288, 34.21857839837574744, -140.2214642502308095 ) ) ;
#8569 = VECTOR ( 'NONE', #10423, 1000.000000000000000 ) ;
#8571 = CIRCLE ( 'NONE', #14674, 2.500000000000000444 ) ;
#8572 = DIRECTION ( 'NONE',  ( -0.09606172499277226828, -0.9953753789357124848, 8.268133652477615271E-13 ) ) ;
#8573 = ORIENTED_EDGE ( 'NONE', *, *, #5987, .F. ) ;
#8574 = CARTESIAN_POINT ( 'NONE',  ( -22.59099198853654400, 37.83876679235774532, -140.4187711903797151 ) ) ;
#8575 = LINE ( 'NONE', #21339, #17716 ) ;
#8576 = CARTESIAN_POINT ( 'NONE',  ( 3.552713678799999608E-15, 50.00000000000000000, -149.5552959529999839 ) ) ;
#8577 = CARTESIAN_POINT ( 'NONE',  ( 7.548835030704958093, 38.16033211785072154, -141.8404982651678097 ) ) ;
#8578 = ORIENTED_EDGE ( 'NONE', *, *, #21161, .F. ) ;
#8579 = CARTESIAN_POINT ( 'NONE',  ( -5.832642628619999492, 38.59814668869999821, -147.7665506369999662 ) ) ;
#8580 = LINE ( 'NONE', #1250, #975 ) ;
#8581 = CARTESIAN_POINT ( 'NONE',  ( -8.937029861356405647, 40.04003061621273218, -145.7935507840504386 ) ) ;
#8582 = CARTESIAN_POINT ( 'NONE',  ( -32.50000000000000000, 26.00000000000000000, -139.5552959529999839 ) ) ;
#8583 = EDGE_CURVE ( 'NONE', #5898, #20128, #14117, .T. ) ;
#8584 = EDGE_LOOP ( 'NONE', ( #21252, #18679, #13870, #3306 ) ) ;
#8585 = ADVANCED_FACE ( 'NONE', ( #1022 ), #8133, .F. ) ;
#8586 = FILL_AREA_STYLE_COLOUR ( '', #12625 ) ;
#8587 = EDGE_LOOP ( 'NONE', ( #11016, #3372, #19710, #5986 ) ) ;
#8588 = AXIS2_PLACEMENT_3D ( 'NONE', #13205, #2294, #2517 ) ;
#8589 = CARTESIAN_POINT ( 'NONE',  ( -7.274215502043762882, 35.55331374630061703, -147.5814222184934863 ) ) ;
#8590 = CYLINDRICAL_SURFACE ( 'NONE', #21839, 2.000000000000001776 ) ;
#8591 = ORIENTED_EDGE ( 'NONE', *, *, #11131, .T. ) ;
#8592 = DIRECTION ( 'NONE',  ( -2.423380700840000070E-27, 0.000000000000000000, -1.000000000000000000 ) ) ;
#8593 = LINE ( 'NONE', #11935, #21690 ) ;
#8594 = ORIENTED_EDGE ( 'NONE', *, *, #19813, .F. ) ;
#8595 = DIRECTION ( 'NONE',  ( -1.000000000000000000, 0.000000000000000000, 0.000000000000000000 ) ) ;
#8596 = DIRECTION ( 'NONE',  ( 4.510774274157260696E-12, -1.321907671014926071E-13, 1.000000000000000000 ) ) ;
#8597 = LINE ( 'NONE', #6831, #15430 ) ;
#8598 = CARTESIAN_POINT ( 'NONE',  ( 12.91075631260000023, -38.04527125359999928, -147.5552959529999839 ) ) ;
#8599 = ADVANCED_FACE ( 'NONE', ( #13859, #8250, #6129, #19208, #4234, #11469, #18748, #2802, #13615, #662, #15173, #8015 ), #15523, .T. ) ;
#8600 = VECTOR ( 'NONE', #21370, 1000.000000000000000 ) ;
#8601 = CARTESIAN_POINT ( 'NONE',  ( 23.50000000000000000, -20.50000000000000000, -137.0552959530000123 ) ) ;
#8602 = VECTOR ( 'NONE', #5807, 1000.000000000000000 ) ;
#8603 = CARTESIAN_POINT ( 'NONE',  ( -17.03115501030000090, 35.19590004879999867, -139.8299307730000010 ) ) ;
#8604 = CARTESIAN_POINT ( 'NONE',  ( 5.961890206001605463, -3.890386884071861395, -150.0552959530000408 ) ) ;
#8605 = DIRECTION ( 'NONE',  ( 0.000000000000000000, 1.000000000000000000, 0.000000000000000000 ) ) ;
#8606 = ORIENTED_EDGE ( 'NONE', *, *, #14919, .F. ) ;
#8607 = LINE ( 'NONE', #15881, #10556 ) ;
#8608 = EDGE_CURVE ( 'NONE', #7053, #2155, #22786, .T. ) ;
#8609 = ORIENTED_EDGE ( 'NONE', *, *, #2845, .F. ) ;
#8610 = ORIENTED_EDGE ( 'NONE', *, *, #22090, .T. ) ;
#8611 = CARTESIAN_POINT ( 'NONE',  ( -15.86078924142569058, 37.04043998682460170, -147.5134597623204229 ) ) ;
#8612 = CARTESIAN_POINT ( 'NONE',  ( -27.84557903575859328, 33.44846360924746165, -141.8624113474437536 ) ) ;
#8613 = ORIENTED_EDGE ( 'NONE', *, *, #21831, .F. ) ;
#8614 = VECTOR ( 'NONE', #11449, 1000.000000000000000 ) ;
#8615 = ORIENTED_EDGE ( 'NONE', *, *, #6957, .T. ) ;
#8616 = DIRECTION ( 'NONE',  ( 0.000000000000000000, 1.603797727360000188E-26, -1.000000000000000000 ) ) ;
#8617 = EDGE_CURVE ( 'NONE', #14599, #7436, #17068, .T. ) ;
#8618 = CARTESIAN_POINT ( 'NONE',  ( -8.613431449180000143, 37.75849558879999535, -140.1079839310000068 ) ) ;
#8619 = AXIS2_PLACEMENT_3D ( 'NONE', #4328, #13123, #5756 ) ;
#8620 = CARTESIAN_POINT ( 'NONE',  ( -12.48399912372551945, 39.13586957977820191, -147.0556079067775954 ) ) ;
#8621 = PLANE ( 'NONE',  #12737 ) ;
#8622 = CARTESIAN_POINT ( 'NONE',  ( -7.946466173734080485, 34.08464986948869324, -140.2285039449382964 ) ) ;
#8623 = ORIENTED_EDGE ( 'NONE', *, *, #9064, .T. ) ;
#8624 = CARTESIAN_POINT ( 'NONE',  ( 9.599503906027615940, 35.97803376242718798, -141.7732779960659570 ) ) ;
#8625 = EDGE_CURVE ( 'NONE', #16505, #8645, #13974, .T. ) ;
#8626 = PLANE ( 'NONE',  #15930 ) ;
#8627 = EDGE_CURVE ( 'NONE', #13656, #22550, #757, .T. ) ;
#8628 = CARTESIAN_POINT ( 'NONE',  ( 3.611688725869999975E-11, 51.50000000000000000, -136.0552959530000123 ) ) ;
#8629 = ORIENTED_EDGE ( 'NONE', *, *, #2136, .F. ) ;
#8630 = EDGE_CURVE ( 'NONE', #11744, #19192, #1734, .T. ) ;
#8631 = EDGE_CURVE ( 'NONE', #34, #21613, #21480, .T. ) ;
#8632 = LINE ( 'NONE', #21163, #21720 ) ;
#8633 = MECHANICAL_DESIGN_GEOMETRIC_PRESENTATION_REPRESENTATION (  '', ( #18914 ), #5239 ) ;
#8634 = VERTEX_POINT ( 'NONE', #4938 ) ;
#8635 = FACE_OUTER_BOUND ( 'NONE', #23193, .T. ) ;
#8636 = CARTESIAN_POINT ( 'NONE',  ( -15.50000000000000000, 21.50000000000000000, -137.0552959530000123 ) ) ;
#8637 = VERTEX_POINT ( 'NONE', #10497 ) ;
#8638 = PLANE ( 'NONE',  #9082 ) ;
#8639 = CARTESIAN_POINT ( 'NONE',  ( -11.76172848620000089, 40.95326072219999958, -146.5101368410000191 ) ) ;
#8640 = VERTEX_POINT ( 'NONE', #21127 ) ;
#8641 = CARTESIAN_POINT ( 'NONE',  ( -21.32113804967662318, 35.98137087654780686, -148.6635683972468200 ) ) ;
#8642 = FACE_OUTER_BOUND ( 'NONE', #5096, .T. ) ;
#8643 = ORIENTED_EDGE ( 'NONE', *, *, #9226, .F. ) ;
#8644 = DIRECTION ( 'NONE',  ( 0.000000000000000000, 0.000000000000000000, 1.000000000000000000 ) ) ;
#8645 = VERTEX_POINT ( 'NONE', #23375 ) ;
#8646 = CARTESIAN_POINT ( 'NONE',  ( 15.50000000000000000, 36.50000000000000000, -136.0552959530000123 ) ) ;
#8647 = CARTESIAN_POINT ( 'NONE',  ( 0.5000000001500000124, 16.89444872450000190, -143.5552959529999839 ) ) ;
#8648 = ORIENTED_EDGE ( 'NONE', *, *, #22457, .F. ) ;
#8649 = CARTESIAN_POINT ( 'NONE',  ( 24.87050155979999744, -26.86223000240000047, -146.0552959529999839 ) ) ;
#8650 = VECTOR ( 'NONE', #644, 1000.000000000000000 ) ;
#8651 = CARTESIAN_POINT ( 'NONE',  ( 3.611688725869999975E-11, 40.00000000000000000, -136.0552959530000123 ) ) ;
#8652 = ORIENTED_EDGE ( 'NONE', *, *, #5752, .F. ) ;
#8653 = CARTESIAN_POINT ( 'NONE',  ( -25.64792992860000354, 37.04465132570000208, -139.7265440090000084 ) ) ;
#8654 = EDGE_CURVE ( 'NONE', #20985, #4528, #2165, .T. ) ;
#8655 = ADVANCED_FACE ( 'NONE', ( #5282 ), #6951, .F. ) ;
#8656 = ORIENTED_EDGE ( 'NONE', *, *, #8331, .F. ) ;
#8657 = PLANE ( 'NONE',  #20399 ) ;
#8658 = PLANE ( 'NONE',  #19956 ) ;
#8659 = CARTESIAN_POINT ( 'NONE',  ( -14.93342499249067679, 39.74098246769964504, -147.8506186731679577 ) ) ;
#8660 = DIRECTION ( 'NONE',  ( 0.000000000000000000, -1.000000000000000000, 0.000000000000000000 ) ) ;
#8661 = VERTEX_POINT ( 'NONE', #19811 ) ;
#8662 = CARTESIAN_POINT ( 'NONE',  ( -7.500000000000000000, 0.000000000000000000, -150.0552959529999839 ) ) ;
#8663 = DIRECTION ( 'NONE',  ( 0.000000000000000000, -1.000000000000000000, 0.000000000000000000 ) ) ;
#8664 = VECTOR ( 'NONE', #12790, 1000.000000000000000 ) ;
#8665 = CARTESIAN_POINT ( 'NONE',  ( 7.200097415480000151, -13.39991276200000136, -143.5552959529999839 ) ) ;
#8666 = VECTOR ( 'NONE', #18524, 1000.000000000000000 ) ;
#8667 = CARTESIAN_POINT ( 'NONE',  ( -28.90798551740000022, 37.01360947639999921, -139.5686590450000040 ) ) ;
#8668 = DIRECTION ( 'NONE',  ( 0.9834926989016489207, 0.1809478134909354718, -4.411697319228424767E-12 ) ) ;
#8669 = LINE ( 'NONE', #9146, #9040 ) ;
#8670 = EDGE_LOOP ( 'NONE', ( #1887, #13574, #9737, #16965 ) ) ;
#8671 = DIRECTION ( 'NONE',  ( -1.000000000000000000, 5.094701932209999624E-24, 2.257144641399999941E-12 ) ) ;
#8672 = CARTESIAN_POINT ( 'NONE',  ( -13.50000000000000711, -42.80076776703756281, -136.0552959529695158 ) ) ;
#8673 = AXIS2_PLACEMENT_3D ( 'NONE', #5715, #7496, #10582 ) ;
#8674 = CARTESIAN_POINT ( 'NONE',  ( -3.500000000000000000, 40.00000000000000000, -150.0552959529999839 ) ) ;
#8675 = CARTESIAN_POINT ( 'NONE',  ( -4.510059210066969193, 37.06110843049351899, -139.6225057176259554 ) ) ;
#8676 = CARTESIAN_POINT ( 'NONE',  ( -8.411849887969999884, 36.09637009080000070, -140.1322081659999981 ) ) ;
#8677 = DIRECTION ( 'NONE',  ( 0.000000000000000000, 2.257144641399999941E-12, 1.000000000000000000 ) ) ;
#8678 = ORIENTED_EDGE ( 'NONE', *, *, #5958, .T. ) ;
#8679 = CARTESIAN_POINT ( 'NONE',  ( 6.500000000040000003, 20.50000000000000000, -136.0552959530000123 ) ) ;
#8680 = PLANE ( 'NONE',  #16289 ) ;
#8681 = ORIENTED_EDGE ( 'NONE', *, *, #104, .T. ) ;
#8682 = VECTOR ( 'NONE', #1911, 1000.000000000000000 ) ;
#8683 = EDGE_CURVE ( 'NONE', #73, #777, #3509, .T. ) ;
#8684 = AXIS2_PLACEMENT_3D ( 'NONE', #4626, #8173, #8294 ) ;
#8685 = ADVANCED_FACE ( 'NONE', ( #12062 ), #21245, .F. ) ;
#8686 = CARTESIAN_POINT ( 'NONE',  ( -29.42801897262304678, 35.14847534977624832, -139.9943774615429390 ) ) ;
#8687 = ORIENTED_EDGE ( 'NONE', *, *, #6128, .F. ) ;
#8688 = VECTOR ( 'NONE', #5943, 1000.000000000000000 ) ;
#8689 = LINE ( 'NONE', #6803, #18211 ) ;
#8690 = DIRECTION ( 'NONE',  ( -2.508215857230000030E-12, 0.000000000000000000, 1.000000000000000000 ) ) ;
#8691 = VECTOR ( 'NONE', #20520, 1000.000000000000000 ) ;
#8692 = CARTESIAN_POINT ( 'NONE',  ( 8.750000000000000000, -42.23606797749999942, -151.0552959529999839 ) ) ;
#8693 = CARTESIAN_POINT ( 'NONE',  ( 7.752982640076552912, 38.30101337195760891, -141.9204103845874556 ) ) ;
#8694 = ORIENTED_EDGE ( 'NONE', *, *, #5736, .T. ) ;
#8695 = CARTESIAN_POINT ( 'NONE',  ( 1.544832289344039822, 26.15117705467530840, -150.0552959529999839 ) ) ;
#8696 = DIRECTION ( 'NONE',  ( -0.06298685227120542907, -0.9980143568310855251, 1.534772309240130738E-13 ) ) ;
#8697 = DIRECTION ( 'NONE',  ( 8.955190032050000935E-12, -9.104778821549999739E-13, 1.000000000000000000 ) ) ;
#8698 = ORIENTED_EDGE ( 'NONE', *, *, #16627, .F. ) ;
#8699 = CYLINDRICAL_SURFACE ( 'NONE', #1602, 2.999999999999999112 ) ;
#8700 = VECTOR ( 'NONE', #11915, 1000.000000000000000 ) ;
#8701 =( NAMED_UNIT ( * ) PLANE_ANGLE_UNIT ( ) SI_UNIT ( $, .RADIAN. ) );
#8702 = VECTOR ( 'NONE', #18923, 1000.000000000000000 ) ;
#8703 = ORIENTED_EDGE ( 'NONE', *, *, #13616, .F. ) ;
#8704 = CARTESIAN_POINT ( 'NONE',  ( -7.179265401243958067, 36.31188407385540273, -147.7652876112470892 ) ) ;
#8705 = CARTESIAN_POINT ( 'NONE',  ( -23.55797472129999903, 40.74841938830000743, -146.3388075610000101 ) ) ;
#8706 = CARTESIAN_POINT ( 'NONE',  ( 22.27731556082403941, -15.33058227694559683, -144.5552959530006945 ) ) ;
#8707 =( BOUNDED_CURVE ( )  B_SPLINE_CURVE ( 5, ( #15083, #16982, #18773, #5494, #466, #13294 ),
 .UNSPECIFIED., .F., .F. ) 
 B_SPLINE_CURVE_WITH_KNOTS ( ( 6, 6 ),
 ( 0.000000000000000000, 1.570796327036584783 ),
 .UNSPECIFIED. ) 
 CURVE ( )  GEOMETRIC_REPRESENTATION_ITEM ( )  RATIONAL_B_SPLINE_CURVE ( ( 1.000000000000000000, 0.5999999999384809657, 0.3999999999384809546, 0.2999999999538607298, 0.2499999999692404939, 0.2500000000000000000 ) ) 
 REPRESENTATION_ITEM ( '' )  );
#8708 = VECTOR ( 'NONE', #8036, 1000.000000000000000 ) ;
#8709 = ORIENTED_EDGE ( 'NONE', *, *, #2275, .F. ) ;
#8710 = VECTOR ( 'NONE', #6749, 1000.000000000000000 ) ;
#8711 = CARTESIAN_POINT ( 'NONE',  ( 4.750000000000000000, -38.23606797749999942, -151.0552959529999839 ) ) ;
#8712 = AXIS2_PLACEMENT_3D ( 'NONE', #9504, #9379, #5945 ) ;
#8713 = DIRECTION ( 'NONE',  ( 0.000000000000000000, -1.000000000000000000, 0.000000000000000000 ) ) ;
#8714 = ORIENTED_EDGE ( 'NONE', *, *, #22483, .F. ) ;
#8715 = CARTESIAN_POINT ( 'NONE',  ( 1.829659965300000080, -16.02499107890000118, -143.5552959529999839 ) ) ;
#8716 = EDGE_CURVE ( 'NONE', #3075, #9674, #18021, .T. ) ;
#8717 = FACE_BOUND ( 'NONE', #22780, .T. ) ;
#8718 = CARTESIAN_POINT ( 'NONE',  ( 0.5000000001409999895, 16.89444872450000190, -147.5552959529999839 ) ) ;
#8719 = EDGE_CURVE ( 'NONE', #17721, #20642, #4755, .T. ) ;
#8720 = CARTESIAN_POINT ( 'NONE',  ( -2.499999999839999987, 31.00000000000000000, -140.5552959529999839 ) ) ;
#8721 = DIRECTION ( 'NONE',  ( 4.430233957459999899E-12, -6.110667527539999876E-13, 1.000000000000000000 ) ) ;
#8722 = FACE_OUTER_BOUND ( 'NONE', #20905, .T. ) ;
#8723 = APPLICATION_PROTOCOL_DEFINITION ( 'draft international standard', 'automotive_design', 1998, #988 ) ;
#8724 = DIRECTION ( 'NONE',  ( 1.000000000000000000, 2.602084704489999637E-17, -1.701177084980000217E-20 ) ) ;
#8725 = VECTOR ( 'NONE', #12401, 1000.000000000000114 ) ;
#8726 = DIRECTION ( 'NONE',  ( 4.510774274159160626E-12, -1.321907670996266040E-13, 1.000000000000000000 ) ) ;
#8727 = AXIS2_PLACEMENT_3D ( 'NONE', #20882, #8008, #15292 ) ;
#8728 = VECTOR ( 'NONE', #19349, 1000.000000000000000 ) ;
#8729 = B_SPLINE_CURVE_WITH_KNOTS ( 'NONE', 3,
 ( #641, #4438, #6459, #11560, #8111, #763, #6107, #9891, #17169, #22643, #8228, #2897, #6336, #22891, #10127, #20989, #6223, #15501 ),
 .UNSPECIFIED., .F., .F.,
 ( 4, 2, 2, 2, 2, 2, 2, 2, 4 ),
 ( 0.000000000000000000, 0.1249999999999999167, 0.2499999999999998335, 0.3749999999999998335, 0.4999999999999998890, 0.6249999999999998890, 0.7499999999999998890, 0.8750000000000000000, 1.000000000000000000 ),
 .UNSPECIFIED. ) ;
#8730 = ORIENTED_EDGE ( 'NONE', *, *, #17551, .F. ) ;
#8731 = CARTESIAN_POINT ( 'NONE',  ( -23.71856152630000025, 38.62313066519999438, -140.3058339320000130 ) ) ;
#8732 = PRODUCT_DEFINITION_CONTEXT ( 'detailed design', #18008, 'design' ) ;
#8733 = ORIENTED_EDGE ( 'NONE', *, *, #14269, .T. ) ;
#8734 = SURFACE_SIDE_STYLE ('',( #1511 ) ) ;
#8735 = ORIENTED_EDGE ( 'NONE', *, *, #3666, .T. ) ;
#8736 = CARTESIAN_POINT ( 'NONE',  ( -15.96502778565563041, 36.28323411072798166, -147.5221219874169947 ) ) ;
#8737 = LINE ( 'NONE', #9844, #15645 ) ;
#8738 = CARTESIAN_POINT ( 'NONE',  ( -32.50000000000000000, 51.00000000000000000, -137.0552959530000123 ) ) ;
#8739 = CARTESIAN_POINT ( 'NONE',  ( -4.499999999949999996, 41.25000000000000000, -150.0552959529999839 ) ) ;
#8740 = VERTEX_POINT ( 'NONE', #12300 ) ;
#8741 = CARTESIAN_POINT ( 'NONE',  ( 25.31684607440000079, 45.26810052420000119, -136.0552959530000123 ) ) ;
#8742 = CARTESIAN_POINT ( 'NONE',  ( -19.14968637899999848, 34.49201595030000078, -147.7870032629999741 ) ) ;
#8743 = LINE ( 'NONE', #12319, #3538 ) ;
#8744 = PLANE ( 'NONE',  #11798 ) ;
#8745 = AXIS2_PLACEMENT_3D ( 'NONE', #1092, #17263, #17620 ) ;
#8746 = EDGE_LOOP ( 'NONE', ( #6065, #19604, #5217, #839 ) ) ;
#8747 = DIRECTION ( 'NONE',  ( -3.781283367744424970E-15, 0.000000000000000000, 1.000000000000000000 ) ) ;
#8748 = VERTEX_POINT ( 'NONE', #15998 ) ;
#8749 = CARTESIAN_POINT ( 'NONE',  ( 9.680021979716793012, 36.07364927583546432, -141.7332369982030116 ) ) ;
#8750 = EDGE_CURVE ( 'NONE', #10047, #16262, #1493, .T. ) ;
#8751 = LINE ( 'NONE', #6738, #365 ) ;
#8752 = LINE ( 'NONE', #8628, #22309 ) ;
#8753 = VERTEX_POINT ( 'NONE', #4081 ) ;
#8754 = PRODUCT_DEFINITION ( 'UNKNOWN', '', #11884, #10159 ) ;
#8755 = ADVANCED_FACE ( 'NONE', ( #13007 ), #14800, .F. ) ;
#8756 = DIRECTION ( 'NONE',  ( 1.526468026909999897E-13, 8.159623473500000156E-13, 1.000000000000000000 ) ) ;
#8757 = ORIENTED_EDGE ( 'NONE', *, *, #5315, .F. ) ;
#8758 = DIRECTION ( 'NONE',  ( 1.000000000000000000, 0.000000000000000000, -4.429789868254375404E-12 ) ) ;
#8759 = AXIS2_PLACEMENT_3D ( 'NONE', #9228, #16495, #18507 ) ;
#8760 = CARTESIAN_POINT ( 'NONE',  ( -32.50000000000000000, 19.50000000000000000, -143.3052959529999839 ) ) ;
#8761 = ORIENTED_EDGE ( 'NONE', *, *, #16598, .F. ) ;
#8762 = DIRECTION ( 'NONE',  ( 1.000000000000000000, 0.000000000000000000, 0.000000000000000000 ) ) ;
#8763 = VERTEX_POINT ( 'NONE', #13118 ) ;
#8764 = CARTESIAN_POINT ( 'NONE',  ( -21.26465617525127527, 34.29107666494682860, -147.5856200583803854 ) ) ;
#8765 = DIRECTION ( 'NONE',  ( 1.000000000000000000, 2.602084704489999637E-17, -1.701177084980000217E-20 ) ) ;
#8766 = EDGE_LOOP ( 'NONE', ( #11872, #13724, #11382, #23272 ) ) ;
#8767 = CARTESIAN_POINT ( 'NONE',  ( 0.000000000000000000, 0.000000000000000000, 0.000000000000000000 ) ) ;
#8768 = EDGE_CURVE ( 'NONE', #21209, #8505, #10978, .T. ) ;
#8769 = ORIENTED_EDGE ( 'NONE', *, *, #9840, .T. ) ;
#8770 = CARTESIAN_POINT ( 'NONE',  ( -26.00874347327740566, 37.97668472797509054, -139.4279068652941191 ) ) ;
#8771 = DIRECTION ( 'NONE',  ( 1.000000000000000000, 0.000000000000000000, 2.507771768020000122E-12 ) ) ;
#8772 = ORIENTED_EDGE ( 'NONE', *, *, #2859, .F. ) ;
#8773 = CARTESIAN_POINT ( 'NONE',  ( 8.500000000050000892, 37.00000000000000000, -146.5552959529999839 ) ) ;
#8774 = EDGE_CURVE ( 'NONE', #18274, #20361, #3737, .T. ) ;
#8775 = DIRECTION ( 'NONE',  ( 2.255140518769847203E-12, 0.000000000000000000, 1.000000000000000000 ) ) ;
#8776 = VERTEX_POINT ( 'NONE', #20389 ) ;
#8777 = CARTESIAN_POINT ( 'NONE',  ( -16.11775386689999934, 33.36946837800000054, -144.2542744049999897 ) ) ;
#8778 = AXIS2_PLACEMENT_3D ( 'NONE', #5390, #12637, #19908 ) ;
#8779 = VECTOR ( 'NONE', #1804, 1000.000000000000000 ) ;
#8780 = VERTEX_POINT ( 'NONE', #20166 ) ;
#8781 = LINE ( 'NONE', #7129, #12795 ) ;
#8782 = CARTESIAN_POINT ( 'NONE',  ( 7.228490359739999427, -13.33508289800000135, -145.5552959529999839 ) ) ;
#8783 = ADVANCED_FACE ( 'NONE', ( #284 ), #16692, .T. ) ;
#8784 = CARTESIAN_POINT ( 'NONE',  ( -13.88298315131738114, 40.45381564898249138, -142.1226073618484520 ) ) ;
#8785 = CARTESIAN_POINT ( 'NONE',  ( -32.50000000000000000, 21.50000000000000000, -150.0552959529999839 ) ) ;
#8786 = EDGE_LOOP ( 'NONE', ( #8921, #16638 ) ) ;
#8787 = CARTESIAN_POINT ( 'NONE',  ( 4.084222279847079307, 13.38246373452060567, -136.0552959530092494 ) ) ;
#8788 = PLANE ( 'NONE',  #5154 ) ;
#8789 = ADVANCED_FACE ( 'NONE', ( #18477 ), #22175, .F. ) ;
#8790 = LINE ( 'NONE', #9143, #15221 ) ;
#8791 = LINE ( 'NONE', #16071, #21275 ) ;
#8792 = LINE ( 'NONE', #23443, #4614 ) ;
#8793 = LINE ( 'NONE', #10695, #20470 ) ;
#8794 =( GEOMETRIC_REPRESENTATION_CONTEXT ( 3 ) GLOBAL_UNCERTAINTY_ASSIGNED_CONTEXT ( ( #1859 ) ) GLOBAL_UNIT_ASSIGNED_CONTEXT ( ( #20777, #4244, #20904 ) ) REPRESENTATION_CONTEXT ( 'NONE', 'WORKASPACE' ) );
#8795 = VERTEX_POINT ( 'NONE', #14452 ) ;
#8796 = AXIS2_PLACEMENT_3D ( 'NONE', #11903, #4419, #9878 ) ;
#8797 = AXIS2_PLACEMENT_3D ( 'NONE', #7860, #18819, #18934 ) ;
#8798 = PRESENTATION_STYLE_ASSIGNMENT (( #1577 ) ) ;
#8799 = EDGE_CURVE ( 'NONE', #10448, #8129, #9300, .T. ) ;
#8800 = CARTESIAN_POINT ( 'NONE',  ( -2.499999999969999998, 40.00000000000000000, -136.5552959530000123 ) ) ;
#8801 = CARTESIAN_POINT ( 'NONE',  ( -12.79720822650000045, 32.99715178900000012, -146.4964997610000239 ) ) ;
#8802 = EDGE_CURVE ( 'NONE', #16549, #13712, #5410, .T. ) ;
#8803 = CARTESIAN_POINT ( 'NONE',  ( -6.183234097860560219, 41.28010592184711669, -143.5033826244076067 ) ) ;
#8804 = CARTESIAN_POINT ( 'NONE',  ( -32.50000000000000000, -35.00000000000000000, -140.0552959529999839 ) ) ;
#8805 = CARTESIAN_POINT ( 'NONE',  ( -9.282104535860000283, -16.71402168319999859, -145.5552959529999839 ) ) ;
#8806 = EDGE_CURVE ( 'NONE', #1178, #5495, #1550, .T. ) ;
#8807 = EDGE_LOOP ( 'NONE', ( #1984, #17604, #4302, #15669, #14090, #7500, #8698, #16036, #12638, #11124, #12711, #20343 ) ) ;
#8808 = LINE ( 'NONE', #12495, #8307 ) ;
#8809 = EDGE_CURVE ( 'NONE', #19622, #1286, #6469, .T. ) ;
#8810 = CARTESIAN_POINT ( 'NONE',  ( -4.192924954330000453, -28.60725908990000121, -145.5552959529999839 ) ) ;
#8811 = VERTEX_POINT ( 'NONE', #16576 ) ;
#8812 = PRODUCT_DEFINITION_SHAPE ( 'NONE', 'NONE',  #8754 ) ;
#8813 = CARTESIAN_POINT ( 'NONE',  ( -30.49999999990000177, 29.00000000000000000, -144.0552959529999839 ) ) ;
#8814 = ORIENTED_EDGE ( 'NONE', *, *, #21981, .T. ) ;
#8815 = LINE ( 'NONE', #19784, #14793 ) ;
#8816 = CARTESIAN_POINT ( 'NONE',  ( -29.76126909798818332, 38.07786601250845138, -139.7317159275528411 ) ) ;
#8817 = CARTESIAN_POINT ( 'NONE',  ( -25.85824191589999899, -34.50000000000000000, -144.8157682190000060 ) ) ;
#8818 = CARTESIAN_POINT ( 'NONE',  ( 7.279327523516623266, 36.12739586069235997, -141.7122832976002371 ) ) ;
#8819 = ORIENTED_EDGE ( 'NONE', *, *, #20012, .F. ) ;
#8820 = CARTESIAN_POINT ( 'NONE',  ( -10.36675979729999852, 34.52853970540000006, -140.3392284379999921 ) ) ;
#8821 = CARTESIAN_POINT ( 'NONE',  ( -18.22769797920763679, 36.96487028399435815, -148.6596776398734789 ) ) ;
#8822 = CARTESIAN_POINT ( 'NONE',  ( -8.780084707271649691, 40.41048401779300292, -144.3937799371521180 ) ) ;
#8823 = CARTESIAN_POINT ( 'NONE',  ( 7.930443943721122935, -30.97545875220255951, -136.0552959530179180 ) ) ;
#8824 = EDGE_LOOP ( 'NONE', ( #4951, #3313, #7728, #13688 ) ) ;
#8825 = CARTESIAN_POINT ( 'NONE',  ( 18.09818317350092798, 24.33939095841219213, -136.0552959530408543 ) ) ;
#8826 = SHAPE_REPRESENTATION_RELATIONSHIP ( 'NONE' , 'NONE' ,  #15746, #1875 ) ;
#8827 = EDGE_CURVE ( 'NONE', #10244, #12707, #16356, .T. ) ;
#8828 = ORIENTED_EDGE ( 'NONE', *, *, #2649, .F. ) ;
#8829 = CYLINDRICAL_SURFACE ( 'NONE', #22492, 2.500000000000002220 ) ;
#8830 = FACE_OUTER_BOUND ( 'NONE', #9036, .T. ) ;
#8831 = CARTESIAN_POINT ( 'NONE',  ( -7.102348325384737926, 25.50000000000001421, -136.0552959529839541 ) ) ;
#8832 = VECTOR ( 'NONE', #20501, 1000.000000000000000 ) ;
#8833 = B_SPLINE_CURVE_WITH_KNOTS ( 'NONE', 3,
 ( #6484, #5160, #21367, #1147, #10496, #21478, #4817, #12061, #13743, #1496, #12406, #19331, #21008, #5057, #12299, #8492, #8378, #19683 ),
 .UNSPECIFIED., .F., .F.,
 ( 4, 2, 2, 2, 2, 2, 2, 2, 4 ),
 ( 0.000000000000000000, 0.1249999999999997224, 0.2499999999999994449, 0.3749999999999991673, 0.4999999999999988898, 0.6249999999999991118, 0.7499999999999994449, 0.8749999999999996669, 1.000000000000000000 ),
 .UNSPECIFIED. ) ;
#8834 = ORIENTED_EDGE ( 'NONE', *, *, #19273, .F. ) ;
#8835 = DIRECTION ( 'NONE',  ( 0.000000000000000000, 0.000000000000000000, 1.000000000000000000 ) ) ;
#8836 = DIRECTION ( 'NONE',  ( 1.000000000000000000, -5.094701932209999624E-24, 0.000000000000000000 ) ) ;
#8837 = EDGE_LOOP ( 'NONE', ( #15261, #18588, #9838, #15070 ) ) ;
#8838 = DIRECTION ( 'NONE',  ( 0.000000000000000000, -1.000000000000000000, 0.000000000000000000 ) ) ;
#8839 = CARTESIAN_POINT ( 'NONE',  ( 19.71905350739518070, 19.57650987475782500, -150.0552959530000123 ) ) ;
#8840 = DIRECTION ( 'NONE',  ( 2.257171095940000041E-12, 1.003664318210000046E-28, 1.000000000000000000 ) ) ;
#8841 = DIRECTION ( 'NONE',  ( 0.000000000000000000, -1.000000000000000000, 0.000000000000000000 ) ) ;
#8842 = DIRECTION ( 'NONE',  ( 0.000000000000000000, 0.000000000000000000, 1.000000000000000000 ) ) ;
#8843 = CARTESIAN_POINT ( 'NONE',  ( -6.072796602490000417, -14.62912504250000012, -143.5552959529999839 ) ) ;
#8844 = PRODUCT_CONTEXT ( 'NONE', #5834, 'mechanical' ) ;
#8845 = CARTESIAN_POINT ( 'NONE',  ( 8.750000000000000000, -38.23606797749999942, -150.0552959529999839 ) ) ;
#8846 = PRESENTATION_LAYER_ASSIGNMENT (  '', '', ( #4296 ) ) ;
#8847 = CARTESIAN_POINT ( 'NONE',  ( -12.28014746100000032, 36.97113097969999984, -148.4919582129999753 ) ) ;
#8848 = LINE ( 'NONE', #5166, #14710 ) ;
#8849 = VERTEX_POINT ( 'NONE', #22061 ) ;
#8850 =( BOUNDED_CURVE ( )  B_SPLINE_CURVE ( 5, ( #23378, #5413, #19464, #3626, #23027, #6834 ),
 .UNSPECIFIED., .F., .F. ) 
 B_SPLINE_CURVE_WITH_KNOTS ( ( 6, 6 ),
 ( 1.570796326654102959, 3.141592653590000062 ),
 .UNSPECIFIED. ) 
 CURVE ( )  GEOMETRIC_REPRESENTATION_ITEM ( )  RATIONAL_B_SPLINE_CURVE ( ( 0.2500000000000000555, 0.2499999999820604335, 0.2999999999730906253, 0.3999999999641208337, 0.5999999999641207893, 1.000000000000000000 ) ) 
 REPRESENTATION_ITEM ( '' )  );
#8851 = ORIENTED_EDGE ( 'NONE', *, *, #10821, .T. ) ;
#8852 =( NAMED_UNIT ( * ) SI_UNIT ( $, .STERADIAN. ) SOLID_ANGLE_UNIT ( ) );
#8853 = EDGE_CURVE ( 'NONE', #7102, #19545, #9863, .T. ) ;
#8854 = VERTEX_POINT ( 'NONE', #9415 ) ;
#8855 = CARTESIAN_POINT ( 'NONE',  ( -16.01154825874916909, 36.06958384727375488, -148.5244474381624400 ) ) ;
#8856 = CARTESIAN_POINT ( 'NONE',  ( 8.750000000030000891, -44.75000000000000000, -136.5552959530000123 ) ) ;
#8857 = EDGE_CURVE ( 'NONE', #16041, #23331, #526, .T. ) ;
#8858 = CARTESIAN_POINT ( 'NONE',  ( 23.19105773460000108, -15.44374190390000123, -146.5552959529999839 ) ) ;
#8859 = DIRECTION ( 'NONE',  ( 2.257749542879999954E-12, 0.000000000000000000, 1.000000000000000000 ) ) ;
#8860 = ORIENTED_EDGE ( 'NONE', *, *, #6702, .F. ) ;
#8861 = FACE_OUTER_BOUND ( 'NONE', #6181, .T. ) ;
#8862 = CARTESIAN_POINT ( 'NONE',  ( -20.06155744032984956, 33.57530910074709141, -142.3227834883446121 ) ) ;
#8863 = CARTESIAN_POINT ( 'NONE',  ( -11.83481770378323716, 38.37786124416315658, -147.4224916050285685 ) ) ;
#8864 = PRODUCT_DEFINITION_FORMATION_WITH_SPECIFIED_SOURCE ( 'ANY', '', #21568, .NOT_KNOWN. ) ;
#8865 = DIRECTION ( 'NONE',  ( 5.094701932209999624E-24, 1.000000000000000000, 0.000000000000000000 ) ) ;
#8866 = ORIENTED_EDGE ( 'NONE', *, *, #8925, .T. ) ;
#8867 = FACE_OUTER_BOUND ( 'NONE', #10656, .T. ) ;
#8868 = VERTEX_POINT ( 'NONE', #12656 ) ;
#8869 = CARTESIAN_POINT ( 'NONE',  ( 9.832297036978788540, 36.31037721551318498, -141.6522196278660033 ) ) ;
#8870 = ADVANCED_FACE ( 'NONE', ( #62 ), #4907, .F. ) ;
#8871 = DIRECTION ( 'NONE',  ( 0.000000000000000000, -2.956752937091289955E-12, -1.000000000000000000 ) ) ;
#8872 = FACE_OUTER_BOUND ( 'NONE', #16918, .T. ) ;
#8873 = ORIENTED_EDGE ( 'NONE', *, *, #12168, .F. ) ;
#8874 = CARTESIAN_POINT ( 'NONE',  ( 20.50000000000000000, -20.50000000000000000, -137.0552959530000123 ) ) ;
#8875 = ORIENTED_EDGE ( 'NONE', *, *, #5617, .F. ) ;
#8876 = CARTESIAN_POINT ( 'NONE',  ( -18.18930989820000121, 36.96028804430000037, -147.6841622079999752 ) ) ;
#8877 = DIRECTION ( 'NONE',  ( 0.000000000000000000, 5.873289694040000105E-29, -1.000000000000000000 ) ) ;
#8878 = ORIENTED_EDGE ( 'NONE', *, *, #9936, .T. ) ;
#8879 = DIRECTION ( 'NONE',  ( -0.1000233216789610108, -0.9949850929136109245, 3.591470555298595137E-13 ) ) ;
#8880 = ORIENTED_EDGE ( 'NONE', *, *, #12655, .F. ) ;
#8881 = EDGE_CURVE ( 'NONE', #4947, #1178, #2843, .T. ) ;
#8882 = VECTOR ( 'NONE', #7298, 1000.000000000000000 ) ;
#8883 = DIRECTION ( 'NONE',  ( 1.000000000000000000, 0.000000000000000000, -4.429789868254374596E-12 ) ) ;
#8884 = CARTESIAN_POINT ( 'NONE',  ( 32.14594224169999848, -40.79958733389999992, -143.0552959529999839 ) ) ;
#8885 = ADVANCED_FACE ( 'NONE', ( #8642 ), #17948, .F. ) ;
#8886 = ORIENTED_EDGE ( 'NONE', *, *, #12755, .T. ) ;
#8887 = VERTEX_POINT ( 'NONE', #21877 ) ;
#8888 = CARTESIAN_POINT ( 'NONE',  ( -27.13199227600000185, 40.71900643419999710, -144.3906906950000177 ) ) ;
#8889 = DIRECTION ( 'NONE',  ( 0.000000000000000000, -1.000000000000000000, 0.000000000000000000 ) ) ;
#8890 = ORIENTED_EDGE ( 'NONE', *, *, #14483, .T. ) ;
#8891 = CARTESIAN_POINT ( 'NONE',  ( 13.13369214870000157, -51.50000000000000000, -136.0552959530000123 ) ) ;
#8892 = DIRECTION ( 'NONE',  ( 2.255973186040000320E-12, 0.000000000000000000, 1.000000000000000000 ) ) ;
#8893 = FACE_OUTER_BOUND ( 'NONE', #21667, .T. ) ;
#8894 = ORIENTED_EDGE ( 'NONE', *, *, #3445, .T. ) ;
#8895 = DIRECTION ( 'NONE',  ( 2.257144641399999941E-12, -4.009147065140000298E-51, 1.000000000000000000 ) ) ;
#8896 = AXIS2_PLACEMENT_3D ( 'NONE', #12144, #983, #1456 ) ;
#8897 = ORIENTED_EDGE ( 'NONE', *, *, #22917, .T. ) ;
#8898 = DIRECTION ( 'NONE',  ( 0.000000000000000000, -1.000000000000000000, 2.257144641399999941E-12 ) ) ;
#8899 = EDGE_CURVE ( 'NONE', #12137, #11748, #21765, .T. ) ;
#8900 = CARTESIAN_POINT ( 'NONE',  ( -46.50000000000000000, 47.50000000000000000, -148.4460207619999892 ) ) ;
#8901 = CARTESIAN_POINT ( 'NONE',  ( -16.45586251408916922, 37.06757768449429591, -140.3467090679593525 ) ) ;
#8902 = CARTESIAN_POINT ( 'NONE',  ( -29.36832786400000117, 38.86294434210000048, -140.8528603229999874 ) ) ;
#8903 = EDGE_LOOP ( 'NONE', ( #4830, #2316 ) ) ;
#8904 = SURFACE_STYLE_FILL_AREA ( #21668 ) ;
#8905 = FACE_OUTER_BOUND ( 'NONE', #3492, .T. ) ;
#8906 = CARTESIAN_POINT ( 'NONE',  ( -16.93971969060000049, -18.00000000000000000, -147.9894163970000136 ) ) ;
#8907 = DIRECTION ( 'NONE',  ( 1.110223024629999900E-16, -1.000000000000000000, 4.148443855749999753E-27 ) ) ;
#8908 = DIRECTION ( 'NONE',  ( -1.000000000000000000, 0.000000000000000000, 0.000000000000000000 ) ) ;
#8909 = CARTESIAN_POINT ( 'NONE',  ( -32.50000000000000000, 10.25000000000000000, -137.0552959530000123 ) ) ;
#8910 = VERTEX_POINT ( 'NONE', #5561 ) ;
#8911 = CARTESIAN_POINT ( 'NONE',  ( 31.50000000000000000, -40.03620104870000063, -136.0552959530000123 ) ) ;
#8912 = CARTESIAN_POINT ( 'NONE',  ( 4.500000000009999113, -3.500000000000000000, -136.0552959530000123 ) ) ;
#8913 = CARTESIAN_POINT ( 'NONE',  ( -12.37691123100000112, 36.07411227369999551, -148.4862478850000116 ) ) ;
#8914 = VECTOR ( 'NONE', #3977, 1000.000000000000000 ) ;
#8915 = CARTESIAN_POINT ( 'NONE',  ( -5.453441311498944621, 40.82075019309078812, -146.2932936048981389 ) ) ;
#8916 = CARTESIAN_POINT ( 'NONE',  ( 3.611688725869999975E-11, 50.50000000000000000, -136.0552959530000123 ) ) ;
#8917 = ORIENTED_EDGE ( 'NONE', *, *, #1498, .T. ) ;
#8918 = CARTESIAN_POINT ( 'NONE',  ( -27.67795712710000089, 37.78351609900000341, -147.6208067679999942 ) ) ;
#8919 = EDGE_CURVE ( 'NONE', #5495, #10871, #19614, .T. ) ;
#8920 = CARTESIAN_POINT ( 'NONE',  ( -16.16113997806631630, 37.07629171513328714, -147.8146678480565868 ) ) ;
#8921 = ORIENTED_EDGE ( 'NONE', *, *, #15465, .T. ) ;
#8922 = CARTESIAN_POINT ( 'NONE',  ( 3.000000000009999113, -3.301139731415996259, -136.0552959530067483 ) ) ;
#8923 = ORIENTED_EDGE ( 'NONE', *, *, #7992, .T. ) ;
#8924 = CARTESIAN_POINT ( 'NONE',  ( 25.31684607480000082, -45.26810052400000473, -150.0552959529999839 ) ) ;
#8925 = EDGE_CURVE ( 'NONE', #18032, #13504, #1894, .T. ) ;
#8926 = LINE ( 'NONE', #3949, #15812 ) ;
#8927 = EDGE_CURVE ( 'NONE', #15926, #23345, #15968, .T. ) ;
#8928 = DIRECTION ( 'NONE',  ( -2.842170943040000002E-14, -3.552713678800000097E-13, -1.000000000000000000 ) ) ;
#8929 = CARTESIAN_POINT ( 'NONE',  ( 7.628223423453324159, 38.22159669780096891, -141.8736084682009277 ) ) ;
#8930 = AXIS2_PLACEMENT_3D ( 'NONE', #9307, #16581, #16471 ) ;
#8931 = EDGE_LOOP ( 'NONE', ( #9130, #917, #7347, #22447, #10098 ) ) ;
#8932 = SURFACE_STYLE_FILL_AREA ( #18001 ) ;
#8933 = CIRCLE ( 'NONE', #994, 3.000000000000000000 ) ;
#8934 = CARTESIAN_POINT ( 'NONE',  ( -19.72358824313251802, 32.72293528688742015, -141.8321840916795793 ) ) ;
#8935 = ADVANCED_FACE ( 'NONE', ( #5094 ), #16043, .F. ) ;
#8936 = CARTESIAN_POINT ( 'NONE',  ( -8.703280531730451131, 40.40219763566103239, -143.6646664510770393 ) ) ;
#8937 = DIRECTION ( 'NONE',  ( 0.000000000000000000, -4.148443855749999753E-27, -1.000000000000000000 ) ) ;
#8938 = EDGE_CURVE ( 'NONE', #3553, #16262, #12578, .T. ) ;
#8939 = EDGE_LOOP ( 'NONE', ( #7986, #10632, #1076, #18039 ) ) ;
#8940 = CARTESIAN_POINT ( 'NONE',  ( 17.88080765324347610, 24.01462304341578147, -136.0552959530404280 ) ) ;
#8941 = SHAPE_REPRESENTATION_RELATIONSHIP ( 'NONE' , 'NONE' ,  #15879, #3845 ) ;
#8942 = EDGE_LOOP ( 'NONE', ( #16208, #18758, #12148, #9972 ) ) ;
#8943 = LINE ( 'NONE', #16224, #81 ) ;
#8944 = DIRECTION ( 'NONE',  ( 1.000000000000000000, 0.000000000000000000, 2.516505522483685870E-12 ) ) ;
#8945 = CARTESIAN_POINT ( 'NONE',  ( -7.101996734191970972, 19.49999999999998579, -136.0552959529840393 ) ) ;
#8946 = VERTEX_POINT ( 'NONE', #12697 ) ;
#8947 = CARTESIAN_POINT ( 'NONE',  ( -4.839510985740364646, 37.75343476009111043, -140.5920901129109950 ) ) ;
#8948 = PLANE ( 'NONE',  #14439 ) ;
#8949 = VECTOR ( 'NONE', #9261, 1000.000000000000000 ) ;
#8950 = VECTOR ( 'NONE', #19185, 1000.000000000000000 ) ;
#8951 = ORIENTED_EDGE ( 'NONE', *, *, #14495, .T. ) ;
#8952 = DIRECTION ( 'NONE',  ( -0.7071067811865463515, 0.7071067811865487940, 1.591319668629388887E-12 ) ) ;
#8953 = B_SPLINE_CURVE_WITH_KNOTS ( 'NONE', 3,
 ( #10667, #21644, #14143, #12337, #10780, #17826, #10545, #1776, #23302, #8997 ),
 .UNSPECIFIED., .F., .F.,
 ( 4, 2, 2, 2, 4 ),
 ( 0.000000000000000000, 0.2500000000000000000, 0.5000000000000000000, 0.7500000000000000000, 1.000000000000000000 ),
 .UNSPECIFIED. ) ;
#8954 = FACE_BOUND ( 'NONE', #184, .T. ) ;
#8955 = DIRECTION ( 'NONE',  ( 4.511946372079999833E-12, -1.314504061159999897E-13, 1.000000000000000000 ) ) ;
#8956 = CARTESIAN_POINT ( 'NONE',  ( -13.18072986969132288, 37.07863008620356027, -148.2345011165225799 ) ) ;
#8957 = ADVANCED_FACE ( 'NONE', ( #12810 ), #14372, .F. ) ;
#8958 = CARTESIAN_POINT ( 'NONE',  ( -15.00000000000000000, -44.50000000000000000, -136.0552959530000123 ) ) ;
#8959 = EDGE_CURVE ( 'NONE', #14486, #4356, #11770, .T. ) ;
#8960 = APPLICATION_PROTOCOL_DEFINITION ( 'draft international standard', 'automotive_design', 1998, #8252 ) ;
#8961 = LINE ( 'NONE', #1855, #23437 ) ;
#8962 = LINE ( 'NONE', #14806, #7026 ) ;
#8963 = CARTESIAN_POINT ( 'NONE',  ( -12.50000000000000000, 22.50000000000000000, -136.0552959530000123 ) ) ;
#8964 = EDGE_LOOP ( 'NONE', ( #4149, #14685, #19803, #8192 ) ) ;
#8965 = CIRCLE ( 'NONE', #2167, 7.000000000000000888 ) ;
#8966 = PRODUCT_DEFINITION_CONTEXT ( 'detailed design', #988, 'design' ) ;
#8967 = ORIENTED_EDGE ( 'NONE', *, *, #13614, .T. ) ;
#8968 = ORIENTED_EDGE ( 'NONE', *, *, #9339, .T. ) ;
#8969 = CARTESIAN_POINT ( 'NONE',  ( -16.37748838231915371, 35.24315528562843980, -148.0100301510570375 ) ) ;
#8970 = CARTESIAN_POINT ( 'NONE',  ( -4.499999999939999995, 31.50000000000000000, -144.0552959529999839 ) ) ;
#8971 = ORIENTED_EDGE ( 'NONE', *, *, #4591, .F. ) ;
#8972 = CARTESIAN_POINT ( 'NONE',  ( 13.76008370044074880, 22.44588062469307488, -136.0552959530310773 ) ) ;
#8973 = ORIENTED_EDGE ( 'NONE', *, *, #19128, .F. ) ;
#8974 = CARTESIAN_POINT ( 'NONE',  ( -22.10824191589999899, -4.000000000000000000, -150.0657682190000060 ) ) ;
#8975 = CARTESIAN_POINT ( 'NONE',  ( 31.32297112069999656, 40.18599471579999971, -149.5552959529999839 ) ) ;
#8976 = CARTESIAN_POINT ( 'NONE',  ( -32.50000000000000000, 27.00000000000000000, -146.5552959529999839 ) ) ;
#8977 = CARTESIAN_POINT ( 'NONE',  ( 4.999999999879999990, -1.500000000000000000, -135.2552959529999725 ) ) ;
#8978 = ORIENTED_EDGE ( 'NONE', *, *, #6957, .F. ) ;
#8979 = FACE_BOUND ( 'NONE', #14716, .T. ) ;
#8980 = VERTEX_POINT ( 'NONE', #23416 ) ;
#8981 = CARTESIAN_POINT ( 'NONE',  ( 9.331285711378725978, 35.75141399242378526, -141.8894180609362650 ) ) ;
#8982 = AXIS2_PLACEMENT_3D ( 'NONE', #9479, #2693, #4030 ) ;
#8983 = EDGE_CURVE ( 'NONE', #14014, #8887, #22421, .T. ) ;
#8984 = DIRECTION ( 'NONE',  ( 1.000000000000000000, 0.000000000000000000, -2.256131789327550371E-12 ) ) ;
#8985 = CARTESIAN_POINT ( 'NONE',  ( -4.959431410700000598, -23.66636161550000139, -146.5552959529999839 ) ) ;
#8986 = ORIENTED_EDGE ( 'NONE', *, *, #7566, .F. ) ;
#8987 = LINE ( 'NONE', #4004, #4599 ) ;
#8988 = ORIENTED_EDGE ( 'NONE', *, *, #2099, .F. ) ;
#8989 = CARTESIAN_POINT ( 'NONE',  ( -20.55139866889999922, 40.46905695040000239, -146.1780460800000014 ) ) ;
#8990 = PLANE ( 'NONE',  #992 ) ;
#8992 = ORIENTED_EDGE ( 'NONE', *, *, #344, .T. ) ;
#8991 = VECTOR ( 'NONE', #14945, 1000.000000000000000 ) ;
#8993 = CARTESIAN_POINT ( 'NONE',  ( -32.50000000000000000, -43.00000000050000182, -137.0552959530000123 ) ) ;
#8994 = ORIENTED_EDGE ( 'NONE', *, *, #15638, .T. ) ;
#8995 = CARTESIAN_POINT ( 'NONE',  ( -16.16113997806634472, 37.07629171513331556, -147.8146678480567004 ) ) ;
#8996 = STYLED_ITEM ( 'NONE', ( #17494 ), #19584 ) ;
#8997 = CARTESIAN_POINT ( 'NONE',  ( -5.500000000000000000, 44.50000000000000000, -150.0552959529999839 ) ) ;
#8998 = ORIENTED_EDGE ( 'NONE', *, *, #16843, .F. ) ;
#8999 = CARTESIAN_POINT ( 'NONE',  ( 0.000000000000000000, 0.000000000000000000, 0.000000000000000000 ) ) ;
#9000 = VERTEX_POINT ( 'NONE', #1421 ) ;
#9001 = CARTESIAN_POINT ( 'NONE',  ( -26.90957831414080914, 39.30870637168261794, -140.7426796967767189 ) ) ;
#9002 = DIRECTION ( 'NONE',  ( 1.000000000000000000, -1.190078432789999897E-50, -2.257144641399999941E-12 ) ) ;
#9003 = VERTEX_POINT ( 'NONE', #23182 ) ;
#9004 = CARTESIAN_POINT ( 'NONE',  ( 10.68320006080000084, -20.50000000000000000, -150.0552959529999839 ) ) ;
#9005 = CARTESIAN_POINT ( 'NONE',  ( -4.888913597060000171, -24.24628707910000003, -142.5552959529999839 ) ) ;
#9006 = FACE_OUTER_BOUND ( 'NONE', #15975, .T. ) ;
#9007 = VERTEX_POINT ( 'NONE', #6875 ) ;
#9008 = EDGE_CURVE ( 'NONE', #13555, #15811, #8953, .T. ) ;
#9009 = AXIS2_PLACEMENT_3D ( 'NONE', #11893, #4529, #4408 ) ;
#9010 = EDGE_CURVE ( 'NONE', #20464, #1248, #3879, .T. ) ;
#9011 = VERTEX_POINT ( 'NONE', #15192 ) ;
#9012 = LINE ( 'NONE', #19519, #15462 ) ;
#9013 = DIRECTION ( 'NONE',  ( -1.000000000000000000, 0.000000000000000000, 2.257120985840000117E-12 ) ) ;
#9014 = CARTESIAN_POINT ( 'NONE',  ( -16.75911775155306316, 38.89720175092567445, -139.8262345698500724 ) ) ;
#9015 = CARTESIAN_POINT ( 'NONE',  ( 32.00000000000000000, 32.96379895120000469, -137.0552959530000123 ) ) ;
#9016 = VERTEX_POINT ( 'NONE', #22448 ) ;
#9017 = DIRECTION ( 'NONE',  ( 1.000000000000000000, 2.602084704489999637E-17, -1.701177084980000217E-20 ) ) ;
#9018 = CARTESIAN_POINT ( 'NONE',  ( -21.35824191589999899, -4.000000000000000000, -146.2257682199999920 ) ) ;
#9019 = FACE_OUTER_BOUND ( 'NONE', #15448, .T. ) ;
#9020 = CARTESIAN_POINT ( 'NONE',  ( -2.499999999839999987, 41.50000000000000000, -139.5552959529999839 ) ) ;
#9021 = CARTESIAN_POINT ( 'NONE',  ( 31.50000000000000000, -2.273736754430000208E-12, -136.0552959530000123 ) ) ;
#9022 = CARTESIAN_POINT ( 'NONE',  ( -22.10824191589999899, -32.00000000000000000, -146.3157682190000060 ) ) ;
#9023 = VERTEX_POINT ( 'NONE', #13049 ) ;
#9024 = CARTESIAN_POINT ( 'NONE',  ( 2.068499633500000545, -14.99362786250000035, -148.5552959529999839 ) ) ;
#9025 = VECTOR ( 'NONE', #15473, 1000.000000000000227 ) ;
#9026 = CARTESIAN_POINT ( 'NONE',  ( -14.24256961507097863, -41.69005684777777532, -136.0552959529678390 ) ) ;
#9027 = CARTESIAN_POINT ( 'NONE',  ( -10.00000000000000000, 48.50000000000000000, -150.0552959529999839 ) ) ;
#9028 = CARTESIAN_POINT ( 'NONE',  ( -5.620151696350735193, 41.14699329952922824, -146.4569507367338588 ) ) ;
#9029 = CARTESIAN_POINT ( 'NONE',  ( -13.86630785130000021, -2.273736754430000208E-12, -136.0552959530000123 ) ) ;
#9030 = ORIENTED_EDGE ( 'NONE', *, *, #12726, .F. ) ;
#9031 = CARTESIAN_POINT ( 'NONE',  ( -14.11967125440000004, 36.98834135279999913, -140.5455248810000057 ) ) ;
#9032 = LINE ( 'NONE', #16319, #12089 ) ;
#9033 = ORIENTED_EDGE ( 'NONE', *, *, #23005, .T. ) ;
#9034 = ADVANCED_FACE ( 'NONE', ( #18643 ), #16856, .F. ) ;
#9035 = CARTESIAN_POINT ( 'NONE',  ( -37.89633983739999934, 26.50000000000000000, -139.8120018070000015 ) ) ;
#9036 = EDGE_LOOP ( 'NONE', ( #17260, #2840, #82, #21830, #18319 ) ) ;
#9037 = DIRECTION ( 'NONE',  ( -0.7633862853691523176, -0.6459422414661291079, 0.000000000000000000 ) ) ;
#9038 = VECTOR ( 'NONE', #20007, 1000.000000000000114 ) ;
#9039 = CARTESIAN_POINT ( 'NONE',  ( -30.43411692010282010, 40.83884358021464323, -144.2352720013742555 ) ) ;
#9040 = VECTOR ( 'NONE', #3460, 1000.000000000000000 ) ;
#9041 = DIRECTION ( 'NONE',  ( -0.9954742291034677226, 0.09503188512734457583, 4.503697062742119365E-12 ) ) ;
#9042 = CARTESIAN_POINT ( 'NONE',  ( 7.113920120768799649, 36.42649308455273882, -141.6219378633786050 ) ) ;
#9043 = ORIENTED_EDGE ( 'NONE', *, *, #684, .T. ) ;
#9044 = CARTESIAN_POINT ( 'NONE',  ( -20.18044358593063947, 35.97457350380363295, -139.5227774015246212 ) ) ;
#9045 = CARTESIAN_POINT ( 'NONE',  ( -8.343166633029998280, 41.26425690090000131, -144.5268661329999986 ) ) ;
#9046 = CARTESIAN_POINT ( 'NONE',  ( 9.724682038211440727, -33.25721777958510472, -136.0552959530218970 ) ) ;
#9047 = VECTOR ( 'NONE', #12940, 1000.000000000000000 ) ;
#9048 = ADVANCED_FACE ( 'NONE', ( #22216 ), #18412, .T. ) ;
#9049 = ORIENTED_EDGE ( 'NONE', *, *, #22956, .T. ) ;
#9050 = DIRECTION ( 'NONE',  ( -0.1146332952500066227, -0.9934078757590583120, -9.710750722050572275E-14 ) ) ;
#9051 = ORIENTED_EDGE ( 'NONE', *, *, #16286, .F. ) ;
#9052 = CARTESIAN_POINT ( 'NONE',  ( -12.50000000000000000, 48.50000000000000000, -150.0552959529999839 ) ) ;
#9053 = PLANE ( 'NONE',  #847 ) ;
#9054 = CARTESIAN_POINT ( 'NONE',  ( -7.499999999959999997, 25.50000000000000000, -136.0552959530000123 ) ) ;
#9055 = CIRCLE ( 'NONE', #22378, 1.000000000000000888 ) ;
#9056 = EDGE_CURVE ( 'NONE', #9183, #22593, #20548, .T. ) ;
#9057 = ORIENTED_EDGE ( 'NONE', *, *, #7628, .T. ) ;
#9058 = DIRECTION ( 'NONE',  ( -0.9892101392001054760, 0.1465035852930155480, 4.471739159800472250E-12 ) ) ;
#9059 = LINE ( 'NONE', #14209, #20155 ) ;
#9060 = AXIS2_PLACEMENT_3D ( 'NONE', #16209, #7155, #10825 ) ;
#9061 = ORIENTED_EDGE ( 'NONE', *, *, #3076, .T. ) ;
#9062 = DIRECTION ( 'NONE',  ( 0.000000000000000000, -2.231104189749999978E-12, 1.000000000000000000 ) ) ;
#9063 = AXIS2_PLACEMENT_3D ( 'NONE', #1336, #13823, #17737 ) ;
#9064 = EDGE_CURVE ( 'NONE', #20852, #7545, #16628, .T. ) ;
#9065 = AXIS2_PLACEMENT_3D ( 'NONE', #13063, #342, #20334 ) ;
#9066 = FACE_BOUND ( 'NONE', #12387, .T. ) ;
#9067 = LINE ( 'NONE', #7525, #4805 ) ;
#9068 = CARTESIAN_POINT ( 'NONE',  ( 1.342750202250000191, -63.28208324180000233, -143.5552959529999839 ) ) ;
#9069 = CARTESIAN_POINT ( 'NONE',  ( 19.50000000000000000, 51.50000000000000000, -137.0552959530000123 ) ) ;
#9070 = CARTESIAN_POINT ( 'NONE',  ( 13.98502865237644777, 39.11890206003842252, -150.0552959529999839 ) ) ;
#9071 = SHAPE_DEFINITION_REPRESENTATION ( #14612, #6152 ) ;
#9072 = LINE ( 'NONE', #1626, #12046 ) ;
#9073 = LINE ( 'NONE', #16246, #8914 ) ;
#9074 = AXIS2_PLACEMENT_3D ( 'NONE', #20984, #759, #7989 ) ;
#9075 = CARTESIAN_POINT ( 'NONE',  ( 1.600095057559999923, -18.40127899619999852, -145.5552959529999839 ) ) ;
#9076 = EDGE_CURVE ( 'NONE', #21875, #1062, #3904, .T. ) ;
#9077 = VERTEX_POINT ( 'NONE', #5790 ) ;
#9078 = ADVANCED_FACE ( 'NONE', ( #13160 ), #20429, .T. ) ;
#9079 = VECTOR ( 'NONE', #14022, 1000.000000000000000 ) ;
#9080 = ORIENTED_EDGE ( 'NONE', *, *, #14904, .F. ) ;
#9081 = SHAPE_REPRESENTATION_RELATIONSHIP ( 'NONE' , 'NONE' ,  #3728, #18583 ) ;
#9082 = AXIS2_PLACEMENT_3D ( 'NONE', #6871, #15913, #10318 ) ;
#9083 = VECTOR ( 'NONE', #8431, 1000.000000000000227 ) ;
#9084 = ORIENTED_EDGE ( 'NONE', *, *, #5963, .F. ) ;
#9085 = LINE ( 'NONE', #3280, #13685 ) ;
#9086 = DIRECTION ( 'NONE',  ( -1.000000000000000000, 0.000000000000000000, 0.000000000000000000 ) ) ;
#9087 = EDGE_LOOP ( 'NONE', ( #9683, #7202, #6796, #11804 ) ) ;
#9088 = DIRECTION ( 'NONE',  ( -0.09606172499277226828, -0.9953753789357124848, 8.268133652477615271E-13 ) ) ;
#9089 = EDGE_CURVE ( 'NONE', #22716, #6049, #4945, .T. ) ;
#9090 = ORIENTED_EDGE ( 'NONE', *, *, #22483, .T. ) ;
#9091 = DIRECTION ( 'NONE',  ( 1.000000000000000000, 0.000000000000000000, -2.262079412673756451E-12 ) ) ;
#9092 = CARTESIAN_POINT ( 'NONE',  ( -19.68771884990000132, 32.54972883539999629, -143.8405663050000101 ) ) ;
#9093 = ADVANCED_FACE ( 'NONE', ( #11136 ), #4123, .F. ) ;
#9094 = CARTESIAN_POINT ( 'NONE',  ( -11.73808716551824638, 40.46300762661749673, -143.7953220469430562 ) ) ;
#9095 = B_SPLINE_CURVE_WITH_KNOTS ( 'NONE', 5,
 ( #16084, #17868, #23453, #11062, #14540, #16545, #255, #20006, #12620, #9160, #8918, #5490 ),
 .UNSPECIFIED., .F., .F.,
 ( 6, 3, 3, 6 ),
 ( 0.000000000000000000, 4.469553974960000176, 8.969854531369998440, 13.50363095830000049 ),
 .UNSPECIFIED. ) ;
#9096 = PLANE ( 'NONE',  #1436 ) ;
#9097 = ORIENTED_EDGE ( 'NONE', *, *, #8207, .T. ) ;
#9098 = FACE_BOUND ( 'NONE', #16325, .T. ) ;
#9099 = ADVANCED_FACE ( 'NONE', ( #16504 ), #9456, .F. ) ;
#9100 = ORIENTED_EDGE ( 'NONE', *, *, #3334, .F. ) ;
#9101 = CARTESIAN_POINT ( 'NONE',  ( 9.039697480175762578, 35.60035037488847109, -141.9838786041871401 ) ) ;
#9102 = AXIS2_PLACEMENT_3D ( 'NONE', #17659, #2797, #21119 ) ;
#9103 = VECTOR ( 'NONE', #16288, 1000.000000000000000 ) ;
#9104 = DIRECTION ( 'NONE',  ( 0.000000000000000000, 0.000000000000000000, 1.000000000000000000 ) ) ;
#9105 = VECTOR ( 'NONE', #4248, 1000.000000000000000 ) ;
#9106 = VECTOR ( 'NONE', #1554, 1000.000000000000000 ) ;
#9107 = CYLINDRICAL_SURFACE ( 'NONE', #9459, 2.000000000000000000 ) ;
#9108 = ORIENTED_EDGE ( 'NONE', *, *, #17344, .T. ) ;
#9109 = LINE ( 'NONE', #2110, #430 ) ;
#9110 = ORIENTED_EDGE ( 'NONE', *, *, #8983, .T. ) ;
#9111 = CARTESIAN_POINT ( 'NONE',  ( 7.976419552961967696, -48.60121046038479875, -150.0552959529999839 ) ) ;
#9112 = DIRECTION ( 'NONE',  ( 1.000000000000000000, 2.602084704489999637E-17, 0.000000000000000000 ) ) ;
#9113 = ORIENTED_EDGE ( 'NONE', *, *, #14325, .F. ) ;
#9114 = CARTESIAN_POINT ( 'NONE',  ( -26.49522641139999735, 37.71913029610000478, -140.3749603070000092 ) ) ;
#9115 = EDGE_LOOP ( 'NONE', ( #18892, #19916, #14462, #22836 ) ) ;
#9116 = CARTESIAN_POINT ( 'NONE',  ( -21.42839884788494231, 35.00147824449854994, -148.3972767829965562 ) ) ;
#9117 = DIRECTION ( 'NONE',  ( 0.000000000000000000, 4.426606872070000353E-37, -1.000000000000000000 ) ) ;
#9118 = ORIENTED_EDGE ( 'NONE', *, *, #5380, .T. ) ;
#9119 = SHAPE_REPRESENTATION_RELATIONSHIP ( 'NONE' , 'NONE' ,  #17559, #18345 ) ;
#9120 = CIRCLE ( 'NONE', #1189, 2.500000000000002220 ) ;
#9121 = AXIS2_PLACEMENT_3D ( 'NONE', #15320, #13285, #18654 ) ;
#9122 = EDGE_CURVE ( 'NONE', #3037, #8645, #11708, .T. ) ;
#9123 = VERTEX_POINT ( 'NONE', #4359 ) ;
#9124 = CARTESIAN_POINT ( 'NONE',  ( -26.69242357735191717, 41.76624275143136344, -143.5162967865278745 ) ) ;
#9125 = EDGE_CURVE ( 'NONE', #232, #11298, #4713, .T. ) ;
#9126 = CARTESIAN_POINT ( 'NONE',  ( -10.69115198329540561, 37.03949207291183399, -140.6562969416297051 ) ) ;
#9127 = DIRECTION ( 'NONE',  ( 2.602084704489999637E-17, -1.000000000000000000, -4.426606872070000353E-37 ) ) ;
#9128 = CARTESIAN_POINT ( 'NONE',  ( 17.58326321919999558, -18.99156222550000095, -146.5552959529999839 ) ) ;
#9129 = DIRECTION ( 'NONE',  ( 0.1051825684329612265, 0.9944529286486342157, 1.406498023189481106E-13 ) ) ;
#9130 = ORIENTED_EDGE ( 'NONE', *, *, #21006, .F. ) ;
#9131 = CARTESIAN_POINT ( 'NONE',  ( 16.13369214859999801, -50.50000000000000000, -137.0552959530000123 ) ) ;
#9132 = LINE ( 'NONE', #14624, #15166 ) ;
#9133 = EDGE_CURVE ( 'NONE', #3527, #751, #17321, .T. ) ;
#9134 = ORIENTED_EDGE ( 'NONE', *, *, #12053, .F. ) ;
#9135 =( GEOMETRIC_REPRESENTATION_CONTEXT ( 3 ) GLOBAL_UNCERTAINTY_ASSIGNED_CONTEXT ( ( #16130 ) ) GLOBAL_UNIT_ASSIGNED_CONTEXT ( ( #6696, #4566, #19193 ) ) REPRESENTATION_CONTEXT ( 'NONE', 'WORKASPACE' ) );
#9136 = PLANE ( 'NONE',  #5204 ) ;
#9137 = CARTESIAN_POINT ( 'NONE',  ( 24.35183050010000017, -28.38413933620000051, -144.5552959529999839 ) ) ;
#9138 = CARTESIAN_POINT ( 'NONE',  ( -17.69601676904985155, 41.72057493329485567, -143.4664273654990154 ) ) ;
#9139 = LINE ( 'NONE', #20105, #22400 ) ;
#9140 = VERTEX_POINT ( 'NONE', #20908 ) ;
#9141 = CARTESIAN_POINT ( 'NONE',  ( -0.009529796579482698038, 16.74243713058401184, -136.0552959529999555 ) ) ;
#9142 = CARTESIAN_POINT ( 'NONE',  ( -34.50000000000000000, -35.00000000000000000, -145.5552959529999839 ) ) ;
#9143 = CARTESIAN_POINT ( 'NONE',  ( 3.421292538029999886, -5.474560764249999600, -135.5552959530000123 ) ) ;
#9144 = CARTESIAN_POINT ( 'NONE',  ( 10.68320006080000084, -19.50000000000000000, -148.5552959529999839 ) ) ;
#9145 = DIRECTION ( 'NONE',  ( -2.602084704489999637E-17, 1.000000000000000000, 4.426606872070000353E-37 ) ) ;
#9146 = CARTESIAN_POINT ( 'NONE',  ( -30.47299999999999898, 15.75516512379999945, -143.0964448760000209 ) ) ;
#9147 = ORIENTED_EDGE ( 'NONE', *, *, #16935, .F. ) ;
#9148 = EDGE_CURVE ( 'NONE', #5769, #7796, #6498, .T. ) ;
#9149 = FACE_OUTER_BOUND ( 'NONE', #23504, .T. ) ;
#9150 = DIRECTION ( 'NONE',  ( -1.000000000000000000, 1.734728570689999873E-18, 2.257171095940000041E-12 ) ) ;
#9151 = EDGE_CURVE ( 'NONE', #17363, #7834, #11595, .T. ) ;
#9152 = PLANE ( 'NONE',  #19343 ) ;
#9153 = CARTESIAN_POINT ( 'NONE',  ( -5.400017929616782730, 41.25700937233216337, -141.5676830613712127 ) ) ;
#9154 = EDGE_CURVE ( 'NONE', #15193, #7436, #17183, .T. ) ;
#9155 = VECTOR ( 'NONE', #5553, 1000.000000000000000 ) ;
#9156 = PLANE ( 'NONE',  #22213 ) ;
#9157 = VECTOR ( 'NONE', #21616, 1000.000000000000000 ) ;
#9158 = AXIS2_PLACEMENT_3D ( 'NONE', #7265, #19769, #1931 ) ;
#9159 = EDGE_LOOP ( 'NONE', ( #22928, #15291, #4634, #20133 ) ) ;
#9160 = CARTESIAN_POINT ( 'NONE',  ( -27.58120011020000106, 38.53525547130000461, -147.4183263870000076 ) ) ;
#9161 = CARTESIAN_POINT ( 'NONE',  ( -9.394779979509999990, -17.86685386420000299, -143.5552959529999839 ) ) ;
#9162 = ORIENTED_EDGE ( 'NONE', *, *, #15268, .F. ) ;
#9163 = ORIENTED_EDGE ( 'NONE', *, *, #15905, .F. ) ;
#9164 = CARTESIAN_POINT ( 'NONE',  ( -24.40630853028789460, 37.68507504038083766, -147.3828018826562243 ) ) ;
#9165 = CARTESIAN_POINT ( 'NONE',  ( -29.80549139627661148, 39.66955698335042513, -141.4168970351647943 ) ) ;
#9166 = CARTESIAN_POINT ( 'NONE',  ( 9.683200060759999062, -20.50000000000000000, -149.3052959529999839 ) ) ;
#9167 = DIRECTION ( 'NONE',  ( 1.000000000000000000, 0.000000000000000000, 2.516505522483685870E-12 ) ) ;
#9168 = ORIENTED_EDGE ( 'NONE', *, *, #6255, .T. ) ;
#9169 = CARTESIAN_POINT ( 'NONE',  ( -35.47299999999999898, 14.00000000000000000, -144.0552959529999839 ) ) ;
#9170 = VECTOR ( 'NONE', #8668, 1000.000000000000114 ) ;
#9171 = CIRCLE ( 'NONE', #22491, 5.000000000000000000 ) ;
#9172 = CARTESIAN_POINT ( 'NONE',  ( -19.92532084487941191, 37.01154022405600585, -139.3892291660192200 ) ) ;
#9173 = VECTOR ( 'NONE', #7836, 1000.000000000000000 ) ;
#9174 = DIRECTION ( 'NONE',  ( 0.000000000000000000, -1.000000000000000000, 1.723073263340000007E-12 ) ) ;
#9175 = CARTESIAN_POINT ( 'NONE',  ( 8.920566648597572978, -31.65725470906492589, -136.0552959530201633 ) ) ;
#9176 = PLANE ( 'NONE',  #17811 ) ;
#9177 = LINE ( 'NONE', #7403, #5371 ) ;
#9178 = EDGE_CURVE ( 'NONE', #8634, #19021, #6373, .T. ) ;
#9179 = DIRECTION ( 'NONE',  ( -0.7633862853691522066, 0.6459422414661292189, -1.795096815436260566E-28 ) ) ;
#9180 = DIRECTION ( 'NONE',  ( 1.000000000000000000, 0.000000000000000000, 0.000000000000000000 ) ) ;
#9181 = EDGE_CURVE ( 'NONE', #4919, #7777, #8395, .T. ) ;
#9182 = FACE_OUTER_BOUND ( 'NONE', #3170, .T. ) ;
#9183 = VERTEX_POINT ( 'NONE', #17570 ) ;
#9184 = CARTESIAN_POINT ( 'NONE',  ( -6.104854084327544506, 39.03903319827616514, -146.8405481461189197 ) ) ;
#9185 = AXIS2_PLACEMENT_3D ( 'NONE', #4739, #707, #8421 ) ;
#9186 = VECTOR ( 'NONE', #15371, 1000.000000000000227 ) ;
#9187 = VERTEX_POINT ( 'NONE', #22805 ) ;
#9188 = VECTOR ( 'NONE', #9465, 1000.000000000000000 ) ;
#9189 = PLANE ( 'NONE',  #6096 ) ;
#9190 = EDGE_CURVE ( 'NONE', #11748, #15992, #22929, .T. ) ;
#9191 = LINE ( 'NONE', #16464, #13639 ) ;
#9192 = CARTESIAN_POINT ( 'NONE',  ( -3.500000000000000000, 44.50000000000000000, -150.0552959529999839 ) ) ;
#9193 = DIRECTION ( 'NONE',  ( 1.000000000000000000, 0.000000000000000000, 0.000000000000000000 ) ) ;
#9194 = DIRECTION ( 'NONE',  ( 1.526468026909860048E-13, 8.159623473498529972E-13, 1.000000000000000000 ) ) ;
#9195 = DIRECTION ( 'NONE',  ( -0.6459422414661291079, 0.7633862853691523176, -2.245315045000450442E-12 ) ) ;
#9196 = CARTESIAN_POINT ( 'NONE',  ( -21.35824191589999899, -32.00000000000000000, -150.0657682190000060 ) ) ;
#9197 = CARTESIAN_POINT ( 'NONE',  ( -2.500000000000000000, 34.00000000000000000, -151.0552959529999839 ) ) ;
#9198 =( BOUNDED_CURVE ( )  B_SPLINE_CURVE ( 5, ( #22415, #22535, #4441, #9895, #8231, #15280 ),
 .UNSPECIFIED., .F., .F. ) 
 B_SPLINE_CURVE_WITH_KNOTS ( ( 6, 6 ),
 ( 1.570796326521524344, 3.141592653590000062 ),
 .UNSPECIFIED. ) 
 CURVE ( )  GEOMETRIC_REPRESENTATION_ITEM ( )  RATIONAL_B_SPLINE_CURVE ( ( 0.2500000000000000000, 0.2499999999651800198, 0.2999999999477699908, 0.3999999999303600062, 0.5999999999303600173, 1.000000000000000000 ) ) 
 REPRESENTATION_ITEM ( '' )  );
#9199 = ADVANCED_FACE ( 'NONE', ( #18871 ), #10169, .T. ) ;
#9200 = PLANE ( 'NONE',  #15496 ) ;
#9201 = ORIENTED_EDGE ( 'NONE', *, *, #4603, .F. ) ;
#9202 = STYLED_ITEM ( 'NONE', ( #3391 ), #10650 ) ;
#9203 = UNCERTAINTY_MEASURE_WITH_UNIT (LENGTH_MEASURE( 1.000000000000000082E-05 ), #21078, 'distance_accuracy_value', 'NONE');
#9204 = AXIS2_PLACEMENT_3D ( 'NONE', #17276, #14179, #1342 ) ;
#9205 = ORIENTED_EDGE ( 'NONE', *, *, #19869, .F. ) ;
#9206 =( NAMED_UNIT ( * ) PLANE_ANGLE_UNIT ( ) SI_UNIT ( $, .RADIAN. ) );
#9207 = VERTEX_POINT ( 'NONE', #4473 ) ;
#9208 = CARTESIAN_POINT ( 'NONE',  ( -17.33409723696195215, 35.21621536416972731, -139.9717982390213251 ) ) ;
#9209 = LINE ( 'NONE', #75, #6138 ) ;
#9210 = ORIENTED_EDGE ( 'NONE', *, *, #16129, .T. ) ;
#9211 = ADVANCED_FACE ( 'NONE', ( #19110 ), #8033, .T. ) ;
#9212 = CARTESIAN_POINT ( 'NONE',  ( 9.824773488100881025, 27.24096059670117853, -136.0552959530222097 ) ) ;
#9213 = ORIENTED_EDGE ( 'NONE', *, *, #19279, .F. ) ;
#9214 = DIRECTION ( 'NONE',  ( -1.000000000000000000, 0.000000000000000000, 2.262368070660000099E-12 ) ) ;
#9215 = CARTESIAN_POINT ( 'NONE',  ( -19.38605492662632201, 35.40602226195235858, -140.5130341973394081 ) ) ;
#9216 = CYLINDRICAL_SURFACE ( 'NONE', #17037, 3.000000000000000000 ) ;
#9217 = ORIENTED_EDGE ( 'NONE', *, *, #16572, .T. ) ;
#9218 = PLANE ( 'NONE',  #14459 ) ;
#9219 = ORIENTED_EDGE ( 'NONE', *, *, #16917, .F. ) ;
#9220 = EDGE_CURVE ( 'NONE', #3556, #15239, #9932, .T. ) ;
#9221 = CARTESIAN_POINT ( 'NONE',  ( 8.598545881123929036, 38.50000000000002132, -142.0552959530002681 ) ) ;
#9222 =( GEOMETRIC_REPRESENTATION_CONTEXT ( 3 ) GLOBAL_UNCERTAINTY_ASSIGNED_CONTEXT ( ( #21137 ) ) GLOBAL_UNIT_ASSIGNED_CONTEXT ( ( #15748, #8701, #3366 ) ) REPRESENTATION_CONTEXT ( 'NONE', 'WORKASPACE' ) );
#9223 = CARTESIAN_POINT ( 'NONE',  ( 9.183200060760000838, -19.50000000000000000, -148.5552959529999839 ) ) ;
#9224 = CARTESIAN_POINT ( 'NONE',  ( -13.86630785140000022, -51.50000000000000000, -136.0552959530000123 ) ) ;
#9225 = ORIENTED_EDGE ( 'NONE', *, *, #23137, .F. ) ;
#9226 = EDGE_CURVE ( 'NONE', #14839, #2120, #920, .T. ) ;
#9227 = ADVANCED_FACE ( 'NONE', ( #15419 ), #22677, .T. ) ;
#9228 = CARTESIAN_POINT ( 'NONE',  ( 18.95053822279999878, 50.00000000000000000, -149.5552959529999839 ) ) ;
#9229 = ORIENTED_EDGE ( 'NONE', *, *, #2166, .F. ) ;
#9230 = DIRECTION ( 'NONE',  ( 3.552713678800000397E-15, 7.105427357600000794E-15, 1.000000000000000000 ) ) ;
#9231 = EDGE_CURVE ( 'NONE', #7230, #15557, #19700, .T. ) ;
#9232 = VERTEX_POINT ( 'NONE', #3523 ) ;
#9233 = CARTESIAN_POINT ( 'NONE',  ( -26.37173218084349458, 38.40595776404164496, -140.8139459235259778 ) ) ;
#9234 = ORIENTED_EDGE ( 'NONE', *, *, #2250, .F. ) ;
#9235 = CARTESIAN_POINT ( 'NONE',  ( -22.46720159712088716, 36.13856230159614569, -139.5983244477151857 ) ) ;
#9236 = EDGE_CURVE ( 'NONE', #23304, #8854, #9085, .T. ) ;
#9237 = ORIENTED_EDGE ( 'NONE', *, *, #18111, .F. ) ;
#9238 = DIRECTION ( 'NONE',  ( 1.000000000000000000, 0.000000000000000000, -4.510774274160000731E-12 ) ) ;
#9239 = AXIS2_PLACEMENT_3D ( 'NONE', #2552, #11213, #20288 ) ;
#9240 = ORIENTED_EDGE ( 'NONE', *, *, #19616, .F. ) ;
#9241 = CARTESIAN_POINT ( 'NONE',  ( 0.000000000000000000, 0.000000000000000000, 0.000000000000000000 ) ) ;
#9242 = ORIENTED_EDGE ( 'NONE', *, *, #21186, .T. ) ;
#9243 = PLANE ( 'NONE',  #14044 ) ;
#9244 = LINE ( 'NONE', #16511, #2657 ) ;
#9245 = DIRECTION ( 'NONE',  ( -0.9836666101882604041, 0.000000000000000000, -0.1800000000020474666 ) ) ;
#9246 = CARTESIAN_POINT ( 'NONE',  ( -6.938784185764151680, 37.04974994750941164, -148.5388410751211268 ) ) ;
#9247 = CARTESIAN_POINT ( 'NONE',  ( -11.01939500368477454, 36.32079862139720206, -140.6910194413075033 ) ) ;
#9248 = PLANE ( 'NONE',  #14005 ) ;
#9249 = ORIENTED_EDGE ( 'NONE', *, *, #22913, .T. ) ;
#9250 = CARTESIAN_POINT ( 'NONE',  ( -3.234790887188633945, 46.50000000000002132, -150.0552959530000408 ) ) ;
#9251 = CARTESIAN_POINT ( 'NONE',  ( 8.962923430288736171, 35.57285519170723376, -146.1079377423460244 ) ) ;
#9252 = VERTEX_POINT ( 'NONE', #16370 ) ;
#9253 = LINE ( 'NONE', #21894, #18876 ) ;
#9254 = FACE_OUTER_BOUND ( 'NONE', #11617, .T. ) ;
#9255 = VECTOR ( 'NONE', #9088, 999.9999999999998863 ) ;
#9256 = EDGE_CURVE ( 'NONE', #11512, #20386, #20610, .T. ) ;
#9257 = CARTESIAN_POINT ( 'NONE',  ( -16.64966033334543738, 38.59029664588182129, -140.5654869318181284 ) ) ;
#9258 = LINE ( 'NONE', #14975, #21271 ) ;
#9259 = EDGE_LOOP ( 'NONE', ( #17354, #17394, #23534, #7709 ) ) ;
#9260 = DIRECTION ( 'NONE',  ( 2.255973186040000320E-12, 0.000000000000000000, 1.000000000000000000 ) ) ;
#9261 = DIRECTION ( 'NONE',  ( -1.000000000000000000, 0.000000000000000000, -2.273736754430000208E-12 ) ) ;
#9262 = LINE ( 'NONE', #12957, #11413 ) ;
#9263 = CARTESIAN_POINT ( 'NONE',  ( -34.50000000000000000, 28.00000000000000000, -144.0552959529999839 ) ) ;
#9264 = LINE ( 'NONE', #13307, #13753 ) ;
#9265 = CARTESIAN_POINT ( 'NONE',  ( 32.50000000000000000, -40.03620104880000241, -142.8052959529999839 ) ) ;
#9266 = ORIENTED_EDGE ( 'NONE', *, *, #14469, .F. ) ;
#9267 = CARTESIAN_POINT ( 'NONE',  ( -28.25100290369999811, 33.74243115720000219, -145.9160084049999853 ) ) ;
#9268 = DIRECTION ( 'NONE',  ( 2.257144641399999941E-12, -8.049635444003269754E-35, 1.000000000000000000 ) ) ;
#9269 = CARTESIAN_POINT ( 'NONE',  ( 23.93638409349999918, -31.59322175579999836, -144.5552959529999839 ) ) ;
#9270 = PLANE ( 'NONE',  #17958 ) ;
#9271 = LINE ( 'NONE', #10580, #13087 ) ;
#9272 = ORIENTED_EDGE ( 'NONE', *, *, #21429, .F. ) ;
#9273 = VECTOR ( 'NONE', #9879, 1000.000000000000000 ) ;
#9274 = DIRECTION ( 'NONE',  ( 0.000000000000000000, 0.000000000000000000, -1.000000000000000000 ) ) ;
#9275 = LINE ( 'NONE', #18103, #16649 ) ;
#9276 = ORIENTED_EDGE ( 'NONE', *, *, #8719, .F. ) ;
#9277 = ORIENTED_EDGE ( 'NONE', *, *, #737, .T. ) ;
#9278 = DIRECTION ( 'NONE',  ( 1.000000000000000000, 0.000000000000000000, 0.000000000000000000 ) ) ;
#9279 = EDGE_CURVE ( 'NONE', #11485, #1998, #6965, .T. ) ;
#9280 = CARTESIAN_POINT ( 'NONE',  ( 13.13369214870000157, 51.50000000000000000, -136.0552959530000123 ) ) ;
#9281 = DIRECTION ( 'NONE',  ( 0.7071067811866730279, -0.3390050494208429743, -0.6205445805637129775 ) ) ;
#9282 = CARTESIAN_POINT ( 'NONE',  ( 8.120291913824591035, 35.54851131638615414, -142.0197959585554202 ) ) ;
#9283 = ORIENTED_EDGE ( 'NONE', *, *, #17841, .T. ) ;
#9284 = CARTESIAN_POINT ( 'NONE',  ( -1.000000000000000000, 20.50000000000000000, -151.0552959529999839 ) ) ;
#9285 = CARTESIAN_POINT ( 'NONE',  ( -19.68771884990000132, 32.54972883539999629, -143.8405663050000101 ) ) ;
#9286 = LINE ( 'NONE', #14555, #22342 ) ;
#9287 = PLANE ( 'NONE',  #15643 ) ;
#9288 = CARTESIAN_POINT ( 'NONE',  ( -22.92066848190323114, 37.01209555897660408, -139.3757315019973930 ) ) ;
#9289 = CARTESIAN_POINT ( 'NONE',  ( 10.17706620004303986, -19.62763245910807797, -148.5552959529999839 ) ) ;
#9290 = CARTESIAN_POINT ( 'NONE',  ( 24.87050155979999744, -26.86223000240000047, -146.5552959529999839 ) ) ;
#9291 = LINE ( 'NONE', #22395, #1989 ) ;
#9292 = FACE_OUTER_BOUND ( 'NONE', #2239, .T. ) ;
#9293 = ORIENTED_EDGE ( 'NONE', *, *, #12139, .T. ) ;
#9294 = CARTESIAN_POINT ( 'NONE',  ( -13.50000000000000000, -43.00000000000000000, -140.0552959529999839 ) ) ;
#9295 = VERTEX_POINT ( 'NONE', #5069 ) ;
#9296 = DIRECTION ( 'NONE',  ( 2.257083409060000051E-12, 0.000000000000000000, 1.000000000000000000 ) ) ;
#9297 = FACE_OUTER_BOUND ( 'NONE', #6991, .T. ) ;
#9299 = AXIS2_PLACEMENT_3D ( 'NONE', #9550, #22646, #6339 ) ;
#9298 = CARTESIAN_POINT ( 'NONE',  ( 1.354168148130000082, -20.95195702430000040, -144.5552959529999839 ) ) ;
#9300 = LINE ( 'NONE', #14571, #3378 ) ;
#9301 = CARTESIAN_POINT ( 'NONE',  ( -13.37265858230000148, 32.83955069500000690, -141.7941727500000013 ) ) ;
#9302 = EDGE_CURVE ( 'NONE', #11634, #8234, #12540, .T. ) ;
#9303 = LINE ( 'NONE', #2196, #7062 ) ;
#9304 = LINE ( 'NONE', #18374, #21947 ) ;
#9305 = CARTESIAN_POINT ( 'NONE',  ( -15.31679993919999916, -34.50000000000000000, -150.0552959529999839 ) ) ;
#9306 = EDGE_CURVE ( 'NONE', #11330, #6049, #19587, .T. ) ;
#9307 = CARTESIAN_POINT ( 'NONE',  ( 4.499999999879999102, -3.000000000000000000, -135.4552959529999896 ) ) ;
#9308 = CARTESIAN_POINT ( 'NONE',  ( 3.000000000010000001, -3.500000000000000000, -136.0552959530000123 ) ) ;
#9309 = ORIENTED_EDGE ( 'NONE', *, *, #18810, .T. ) ;
#9310 = ORIENTED_EDGE ( 'NONE', *, *, #23058, .F. ) ;
#9311 =( NAMED_UNIT ( * ) SI_UNIT ( $, .STERADIAN. ) SOLID_ANGLE_UNIT ( ) );
#9312 = ORIENTED_EDGE ( 'NONE', *, *, #22222, .F. ) ;
#9313 = AXIS2_PLACEMENT_3D ( 'NONE', #19438, #3246, #10479 ) ;
#9314 = LINE ( 'NONE', #18276, #17165 ) ;
#9315 = CARTESIAN_POINT ( 'NONE',  ( -9.072898850179999641, 36.94639249900000522, -148.2684494029999769 ) ) ;
#9316 = VECTOR ( 'NONE', #18632, 1000.000000000000000 ) ;
#9317 = DIRECTION ( 'NONE',  ( -0.9934078757590584230, 0.1146332952500066366, 4.471042303700267278E-12 ) ) ;
#9318 = ORIENTED_EDGE ( 'NONE', *, *, #3440, .F. ) ;
#9319 = CARTESIAN_POINT ( 'NONE',  ( 25.11919234684406277, 34.98537695656359858, -136.0552959530567421 ) ) ;
#9320 = LINE ( 'NONE', #20529, #14064 ) ;
#9321 = FACE_OUTER_BOUND ( 'NONE', #6016, .T. ) ;
#9322 = ORIENTED_EDGE ( 'NONE', *, *, #18117, .T. ) ;
#9323 = CARTESIAN_POINT ( 'NONE',  ( -19.59255166816691940, 37.05126161860788159, -140.3061871180788103 ) ) ;
#9324 = ADVANCED_FACE ( 'NONE', ( #10752, #4954 ), #12423, .F. ) ;
#9325 = CARTESIAN_POINT ( 'NONE',  ( 18.18320006080000084, 0.4999999999990000776, -150.0552959529999839 ) ) ;
#9326 =( BOUNDED_SURFACE ( )  B_SPLINE_SURFACE ( 5, 5, ( 
 ( #15503, #6338, #889, #6576, #8473, #4681 ),
 ( #10012, #5036, #6690, #1125, #19551, #6461 ),
 ( #15386, #21343, #13594, #4561, #11799, #17289 ),
 ( #4797, #2785, #15851, #1001, #13950, #19310 ),
 ( #12162, #8230, #21223, #22763, #13719, #19435 ),
 ( #3139, #2899, #10369, #20991, #23118, #11923 ),
 ( #19189, #10129, #17404, #10831, #15976, #10720 ),
 ( #23236, #21817, #10953, #12634, #155, #7398 ),
 ( #14305, #14659, #40, #7162, #14428, #8820 ),
 ( #5610, #1473, #21928, #14553, #21576, #1599 ),
 ( #5258, #12509, #6931, #12747, #3715, #19790 ),
 ( #23466, #5501, #23353, #14192, #16096, #21699 ) ),
 .UNSPECIFIED., .F., .F., .F. ) 
 B_SPLINE_SURFACE_WITH_KNOTS ( ( 6, 3, 3, 6 ),
 ( 6, 6 ),
 ( 0.000000000000000000, 4.570086947620000117, 8.869210483019999813, 12.91901055009999943 ),
 ( 1.570796326400424991, 3.141592653590000062 ),
 .UNSPECIFIED. ) 
 GEOMETRIC_REPRESENTATION_ITEM ( )  RATIONAL_B_SPLINE_SURFACE ( (
 ( 0.2500000000000000000, 0.2499999999497609926, 0.2999999999246414917, 0.3999999998995225070, 0.5999999998995220185, 1.000000000000000000),
 ( 0.2500000000000000000, 0.2499999999497609926, 0.2999999999246414917, 0.3999999998995225070, 0.5999999998995220185, 1.000000000000000000),
 ( 0.2500000000000000000, 0.2499999999497609926, 0.2999999999246414917, 0.3999999998995225070, 0.5999999998995220185, 1.000000000000000000),
 ( 0.2500000000000000000, 0.2499999999497609926, 0.2999999999246414917, 0.3999999998995225070, 0.5999999998995220185, 1.000000000000000000),
 ( 0.2500000000000000000, 0.2499999999497609926, 0.2999999999246414917, 0.3999999998995225070, 0.5999999998995220185, 1.000000000000000000),
 ( 0.2500000000000000000, 0.2499999999497609926, 0.2999999999246414917, 0.3999999998995225070, 0.5999999998995220185, 1.000000000000000000),
 ( 0.2500000000000000000, 0.2499999999497609926, 0.2999999999246414917, 0.3999999998995225070, 0.5999999998995220185, 1.000000000000000000),
 ( 0.2500000000000000000, 0.2499999999497609926, 0.2999999999246414917, 0.3999999998995225070, 0.5999999998995220185, 1.000000000000000000),
 ( 0.2500000000000000000, 0.2499999999497609926, 0.2999999999246414917, 0.3999999998995225070, 0.5999999998995220185, 1.000000000000000000),
 ( 0.2500000000000000000, 0.2499999999497609926, 0.2999999999246414917, 0.3999999998995225070, 0.5999999998995220185, 1.000000000000000000),
 ( 0.2500000000000000000, 0.2499999999497609926, 0.2999999999246414917, 0.3999999998995225070, 0.5999999998995220185, 1.000000000000000000),
 ( 0.2500000000000000000, 0.2499999999497609926, 0.2999999999246414917, 0.3999999998995225070, 0.5999999998995220185, 1.000000000000000000) ) ) 
 REPRESENTATION_ITEM ( '' )  SURFACE ( )  );
#9327 = LINE ( 'NONE', #7221, #17315 ) ;
#9328 = VECTOR ( 'NONE', #13301, 1000.000000000000000 ) ;
#9329 = CARTESIAN_POINT ( 'NONE',  ( -24.10813950037725206, 36.95059904178096133, -147.5089432696950382 ) ) ;
#9330 = VECTOR ( 'NONE', #8690, 1000.000000000000000 ) ;
#9331 = VERTEX_POINT ( 'NONE', #16251 ) ;
#9332 = CARTESIAN_POINT ( 'NONE',  ( 7.795574410691926026, -18.05719095672263563, -147.5552959530097894 ) ) ;
#9333 = ORIENTED_EDGE ( 'NONE', *, *, #20130, .F. ) ;
#9334 = CARTESIAN_POINT ( 'NONE',  ( 6.500000000030000002, 13.00000000000000000, -137.0552959530000123 ) ) ;
#9335 = EDGE_LOOP ( 'NONE', ( #9369, #6347, #18737, #9394 ) ) ;
#9336 = CARTESIAN_POINT ( 'NONE',  ( -25.48612782046226144, 37.91366991941922748, -140.0433563333232314 ) ) ;
#9337 = ORIENTED_EDGE ( 'NONE', *, *, #4059, .T. ) ;
#9338 = CARTESIAN_POINT ( 'NONE',  ( 18.95053822279999878, -50.50000000000000000, -150.0552959529999839 ) ) ;
#9339 = EDGE_CURVE ( 'NONE', #14260, #23322, #14466, .T. ) ;
#9340 = ORIENTED_EDGE ( 'NONE', *, *, #16151, .T. ) ;
#9341 = CARTESIAN_POINT ( 'NONE',  ( -12.37864083493721878, -44.51085694111268509, -150.0552959529999839 ) ) ;
#9342 = ORIENTED_EDGE ( 'NONE', *, *, #23303, .T. ) ;
#9343 =( NAMED_UNIT ( * ) PLANE_ANGLE_UNIT ( ) SI_UNIT ( $, .RADIAN. ) );
#9344 = ORIENTED_EDGE ( 'NONE', *, *, #6327, .F. ) ;
#9345 = CARTESIAN_POINT ( 'NONE',  ( -27.58120011020000106, 38.53525547130000461, -147.4183263870000076 ) ) ;
#9346 = CARTESIAN_POINT ( 'NONE',  ( -23.81889237380000068, 39.38287674749999923, -140.7489234159999967 ) ) ;
#9347 = CIRCLE ( 'NONE', #15822, 8.000000000000000000 ) ;
#9348 = CARTESIAN_POINT ( 'NONE',  ( -46.29070078880000239, 29.00000000000000000, -147.5552959540000018 ) ) ;
#9349 = PLANE ( 'NONE',  #2616 ) ;
#9350 = DIRECTION ( 'NONE',  ( 0.7071067811865475727, 0.7071067811865475727, 0.000000000000000000 ) ) ;
#9351 = ADVANCED_FACE ( 'NONE', ( #19477 ), #18150, .F. ) ;
#9352 = CARTESIAN_POINT ( 'NONE',  ( -32.50000000000000000, 50.00000000000000000, -151.0552959529999839 ) ) ;
#9353 = ORIENTED_EDGE ( 'NONE', *, *, #7438, .T. ) ;
#9354 = ADVANCED_FACE ( 'NONE', ( #74 ), #3171, .F. ) ;
#9355 = CARTESIAN_POINT ( 'NONE',  ( 6.500000000149999124, 20.50000000000000000, -143.5552959529999839 ) ) ;
#9356 = EDGE_CURVE ( 'NONE', #15779, #20935, #1388, .T. ) ;
#9357 = DIRECTION ( 'NONE',  ( 0.000000000000000000, -1.000000000000000000, 0.000000000000000000 ) ) ;
#9358 = ADVANCED_FACE ( 'NONE', ( #5424 ), #7339, .F. ) ;
#9359 = ORIENTED_EDGE ( 'NONE', *, *, #8103, .T. ) ;
#9360 = DIRECTION ( 'NONE',  ( -1.000000000000000000, 0.000000000000000000, 0.000000000000000000 ) ) ;
#9361 = AXIS2_PLACEMENT_3D ( 'NONE', #11796, #22412, #18952 ) ;
#9362 = CARTESIAN_POINT ( 'NONE',  ( -12.82596392966510379, 39.28888178912641393, -147.2049309481724038 ) ) ;
#9363 = CARTESIAN_POINT ( 'NONE',  ( -16.55393100702923093, 37.83050752194322541, -140.3603090961101429 ) ) ;
#9364 = CARTESIAN_POINT ( 'NONE',  ( 3.611688725869999975E-11, 19.50000000000000000, -136.0552959530000123 ) ) ;
#9365 = VECTOR ( 'NONE', #17783, 1000.000000000000000 ) ;
#9366 = ORIENTED_EDGE ( 'NONE', *, *, #417, .F. ) ;
#9367 = CARTESIAN_POINT ( 'NONE',  ( -20.60824191589999899, -4.000000000000000000, -146.2257682199999920 ) ) ;
#9368 = DIRECTION ( 'NONE',  ( -2.508215857230000030E-12, 0.000000000000000000, 1.000000000000000000 ) ) ;
#9369 = ORIENTED_EDGE ( 'NONE', *, *, #14244, .F. ) ;
#9370 = DIRECTION ( 'NONE',  ( 1.000000000000000000, 2.602084704489999637E-17, -1.701177084980000217E-20 ) ) ;
#9371 = DIRECTION ( 'NONE',  ( -0.9874789572432817186, 0.1577507813030449846, 2.125043109900604696E-14 ) ) ;
#9372 = DIRECTION ( 'NONE',  ( 0.000000000000000000, -1.000000000000000000, 0.000000000000000000 ) ) ;
#9373 = CARTESIAN_POINT ( 'NONE',  ( -20.72654659758507378, 41.81248471335479877, -143.6178682002461926 ) ) ;
#9374 = ORIENTED_EDGE ( 'NONE', *, *, #23081, .T. ) ;
#9375 = CARTESIAN_POINT ( 'NONE',  ( -27.26567793390747596, 36.96940380712532459, -148.4835048638151989 ) ) ;
#9376 = LINE ( 'NONE', #3820, #18266 ) ;
#9377 = LINE ( 'NONE', #22139, #15928 ) ;
#9378 = DIRECTION ( 'NONE',  ( 0.000000000000000000, 0.000000000000000000, 1.000000000000000000 ) ) ;
#9379 = DIRECTION ( 'NONE',  ( 2.839308199620000013E-14, 3.568879590630000244E-13, 1.000000000000000000 ) ) ;
#9380 = VECTOR ( 'NONE', #7159, 1000.000000000000000 ) ;
#9381 = ORIENTED_EDGE ( 'NONE', *, *, #23005, .F. ) ;
#9382 = EDGE_CURVE ( 'NONE', #10546, #22041, #2251, .T. ) ;
#9383 = CARTESIAN_POINT ( 'NONE',  ( -32.50000000000000000, -36.00000000000000000, -143.3052959529999839 ) ) ;
#9384 = EDGE_CURVE ( 'NONE', #23125, #1659, #7558, .T. ) ;
#9385 = VECTOR ( 'NONE', #16671, 1000.000000000000000 ) ;
#9386 = LINE ( 'NONE', #16661, #6384 ) ;
#9387 = ORIENTED_EDGE ( 'NONE', *, *, #1797, .T. ) ;
#9388 = ADVANCED_FACE ( 'NONE', ( #11655 ), #18933, .F. ) ;
#9389 = ORIENTED_EDGE ( 'NONE', *, *, #18564, .T. ) ;
#9390 = CARTESIAN_POINT ( 'NONE',  ( -22.39162803485939079, 36.31163189668782820, -140.3928250950291101 ) ) ;
#9391 = LINE ( 'NONE', #18699, #10043 ) ;
#9392 = CARTESIAN_POINT ( 'NONE',  ( -32.50000000000000000, -14.25000000000000000, -150.0552959529999839 ) ) ;
#9393 = CARTESIAN_POINT ( 'NONE',  ( 8.188105526302459580, 35.53272852138334059, -142.0311810631520757 ) ) ;
#9394 = ORIENTED_EDGE ( 'NONE', *, *, #16522, .F. ) ;
#9395 = CARTESIAN_POINT ( 'NONE',  ( 32.00000000000000000, -39.80430157320000006, -149.5552959529999839 ) ) ;
#9396 = CARTESIAN_POINT ( 'NONE',  ( -19.21862483442529523, 34.19907101541957672, -140.3476381199748744 ) ) ;
#9397 = AXIS2_PLACEMENT_3D ( 'NONE', #3745, #9422, #16699 ) ;
#9398 = CARTESIAN_POINT ( 'NONE',  ( -25.85824191589999899, -1.500000000000000000, -144.8157682190000060 ) ) ;
#9399 = DIRECTION ( 'NONE',  ( 1.526468026909999897E-13, 8.159623473500000156E-13, 1.000000000000000000 ) ) ;
#9400 = CARTESIAN_POINT ( 'NONE',  ( -23.84605196395386884, 41.80962803837999786, -144.6368725230021255 ) ) ;
#9401 = AXIS2_PLACEMENT_3D ( 'NONE', #14041, #7257, #5358 ) ;
#9402 = CARTESIAN_POINT ( 'NONE',  ( -15.90559286389999905, 34.15404988380000617, -147.7469703310000000 ) ) ;
#9403 = CARTESIAN_POINT ( 'NONE',  ( -19.57725164000000007, 32.58775676329999271, -144.7853266960000269 ) ) ;
#9404 = CARTESIAN_POINT ( 'NONE',  ( 4.500000000009999113, -5.000000000000000000, -136.5552959530000123 ) ) ;
#9405 = DIRECTION ( 'NONE',  ( 0.000000000000000000, -7.444689577964079813E-14, -1.000000000000000000 ) ) ;
#9406 = VERTEX_POINT ( 'NONE', #8211 ) ;
#9407 = EDGE_CURVE ( 'NONE', #21983, #1038, #2877, .T. ) ;
#9408 = CARTESIAN_POINT ( 'NONE',  ( -5.024157003614323713, 39.12743904224282687, -141.1587107399263914 ) ) ;
#9409 = ADVANCED_FACE ( 'NONE', ( #6788 ), #5122, .F. ) ;
#9410 = VERTEX_POINT ( 'NONE', #8453 ) ;
#9411 = CARTESIAN_POINT ( 'NONE',  ( -7.129475577410000042, -25.57825421080000083, -143.5552959529999839 ) ) ;
#9412 = VECTOR ( 'NONE', #21804, 1000.000000000000000 ) ;
#9413 = MECHANICAL_DESIGN_GEOMETRIC_PRESENTATION_REPRESENTATION (  '', ( #4114 ), #18171 ) ;
#9414 = CARTESIAN_POINT ( 'NONE',  ( -22.17914504452174640, 36.26149632490731989, -147.8500484283999299 ) ) ;
#9415 = CARTESIAN_POINT ( 'NONE',  ( 8.900000000049999471, 34.53220746410000430, -148.7552959530000010 ) ) ;
#9416 = ORIENTED_EDGE ( 'NONE', *, *, #1826, .T. ) ;
#9417 = CARTESIAN_POINT ( 'NONE',  ( -12.34038114069202585, 33.41076594416544765, -146.1814057331143886 ) ) ;
#9418 = CARTESIAN_POINT ( 'NONE',  ( 22.50000000000000000, 33.50000000000000000, -136.5552959530000123 ) ) ;
#9419 = LINE ( 'NONE', #1854, #18888 ) ;
#9420 = DIRECTION ( 'NONE',  ( 0.000000000000000000, -1.000000000000000000, 0.000000000000000000 ) ) ;
#9421 = LINE ( 'NONE', #22181, #17288 ) ;
#9422 = DIRECTION ( 'NONE',  ( 2.257144641399999941E-12, -4.009147065140000298E-51, 1.000000000000000000 ) ) ;
#9423 = ORIENTED_EDGE ( 'NONE', *, *, #2549, .F. ) ;
#9424 = CARTESIAN_POINT ( 'NONE',  ( 5.749999999879999102, -4.000000000000000000, -135.0552959530000123 ) ) ;
#9425 = ORIENTED_EDGE ( 'NONE', *, *, #17606, .F. ) ;
#9426 = AXIS2_PLACEMENT_3D ( 'NONE', #18210, #3816, #19994 ) ;
#9427 = ORIENTED_EDGE ( 'NONE', *, *, #8364, .T. ) ;
#9428 = CARTESIAN_POINT ( 'NONE',  ( -13.21931118272387984, 33.83281470431867888, -146.0365350581830057 ) ) ;
#9429 = CARTESIAN_POINT ( 'NONE',  ( -18.35824191589999899, -34.50000000000000000, -144.8157682190000060 ) ) ;
#9430 = DIRECTION ( 'NONE',  ( 1.000000000000000000, 0.000000000000000000, 0.000000000000000000 ) ) ;
#9431 = AXIS2_PLACEMENT_3D ( 'NONE', #11361, #13275, #7799 ) ;
#9432 = ORIENTED_EDGE ( 'NONE', *, *, #21916, .T. ) ;
#9433 = EDGE_CURVE ( 'NONE', #20938, #8241, #21322, .T. ) ;
#9434 = VECTOR ( 'NONE', #16201, 1000.000000000000114 ) ;
#9435 = CARTESIAN_POINT ( 'NONE',  ( -8.916553640509999212, -11.88594259849999979, -143.0552959529999839 ) ) ;
#9436 = DIRECTION ( 'NONE',  ( 0.000000000000000000, 2.259525899700000234E-12, 1.000000000000000000 ) ) ;
#9437 = EDGE_CURVE ( 'NONE', #11594, #467, #12368, .T. ) ;
#9438 = DIRECTION ( 'NONE',  ( 0.4293832457559224602, -0.9031223772358367707, 6.707597440443650396E-13 ) ) ;
#9439 = VERTEX_POINT ( 'NONE', #15721 ) ;
#9440 = CARTESIAN_POINT ( 'NONE',  ( -20.07993885570694559, 39.12723785091482398, -141.2403607577224420 ) ) ;
#9441 = CARTESIAN_POINT ( 'NONE',  ( 9.843919113198380089, 37.66802811340684798, -141.6458064975830951 ) ) ;
#9442 = VECTOR ( 'NONE', #15211, 1000.000000000000000 ) ;
#9443 = CARTESIAN_POINT ( 'NONE',  ( -18.07392865170000107, -1.500000000000000000, -145.5657682190000060 ) ) ;
#9444 = VECTOR ( 'NONE', #13507, 1000.000000000000227 ) ;
#9445 = LINE ( 'NONE', #16724, #20783 ) ;
#9446 = ORIENTED_EDGE ( 'NONE', *, *, #20582, .F. ) ;
#9447 = AXIS2_PLACEMENT_3D ( 'NONE', #21683, #11171, #18217 ) ;
#9448 = VECTOR ( 'NONE', #17281, 1000.000000000000000 ) ;
#9449 = DIRECTION ( 'NONE',  ( -1.000000000000000000, 0.000000000000000000, 0.000000000000000000 ) ) ;
#9450 = VERTEX_POINT ( 'NONE', #14175 ) ;
#9451 = EDGE_LOOP ( 'NONE', ( #17121, #2054, #16150, #22839, #15413, #3348 ) ) ;
#9452 = CARTESIAN_POINT ( 'NONE',  ( -27.03718401022160478, 40.11783903597983425, -145.8300916363254203 ) ) ;
#9453 = ORIENTED_EDGE ( 'NONE', *, *, #7207, .T. ) ;
#9454 = CARTESIAN_POINT ( 'NONE',  ( -22.04078958492209850, 33.03316129315219740, -141.6299626085071566 ) ) ;
#9455 = VERTEX_POINT ( 'NONE', #6437 ) ;
#9456 = PLANE ( 'NONE',  #21293 ) ;
#9457 = ORIENTED_EDGE ( 'NONE', *, *, #1643, .T. ) ;
#9458 = APPLICATION_PROTOCOL_DEFINITION ( 'draft international standard', 'automotive_design', 1998, #2653 ) ;
#9459 = AXIS2_PLACEMENT_3D ( 'NONE', #3417, #12685, #19952 ) ;
#9460 = ORIENTED_EDGE ( 'NONE', *, *, #9384, .F. ) ;
#9461 = CARTESIAN_POINT ( 'NONE',  ( -28.90798551740000022, 37.01360947639999921, -139.5686590450000040 ) ) ;
#9462 = APPLICATION_CONTEXT ( 'automotive_design' ) ;
#9463 = AXIS2_PLACEMENT_3D ( 'NONE', #13839, #6224, #1247 ) ;
#9464 = DIRECTION ( 'NONE',  ( 0.000000000000000000, -1.000000000000000000, 0.000000000000000000 ) ) ;
#9465 = DIRECTION ( 'NONE',  ( -8.955280961229999814E-12, 9.094947017729999296E-13, -1.000000000000000000 ) ) ;
#9466 = EDGE_CURVE ( 'NONE', #10468, #12804, #22870, .T. ) ;
#9467 = DIRECTION ( 'NONE',  ( -1.082120504314331458E-12, 0.8775825618903714265, -0.4794255386042053368 ) ) ;
#9468 = AXIS2_PLACEMENT_3D ( 'NONE', #8646, #4635, #6879 ) ;
#9469 = CARTESIAN_POINT ( 'NONE',  ( -7.107905118430739577, 36.22301459085688435, -148.1570340886389943 ) ) ;
#9470 = VECTOR ( 'NONE', #13186, 1000.000000000000000 ) ;
#9471 = CARTESIAN_POINT ( 'NONE',  ( 10.50000000020000002, 16.50000000000000000, -136.5552959530000123 ) ) ;
#9472 = EDGE_LOOP ( 'NONE', ( #7849, #962, #9266, #10081 ) ) ;
#9473 = DIRECTION ( 'NONE',  ( -1.000000000000000000, 0.000000000000000000, 2.257144641399999941E-12 ) ) ;
#9474 = PRODUCT_RELATED_PRODUCT_CATEGORY ( 'part', '', ( #1896 ) ) ;
#9475 = CARTESIAN_POINT ( 'NONE',  ( 14.00000000000000000, 20.50000000000000000, -150.5552959529999839 ) ) ;
#9476 = ADVANCED_FACE ( 'NONE', ( #15957 ), #21438, .F. ) ;
#9477 = CARTESIAN_POINT ( 'NONE',  ( -15.00000000000000000, -41.50000000000000000, -136.5552959530000123 ) ) ;
#9478 = ORIENTED_EDGE ( 'NONE', *, *, #16103, .F. ) ;
#9479 = CARTESIAN_POINT ( 'NONE',  ( 13.13369214859999978, -51.50000000000000000, -137.0552959530000123 ) ) ;
#9480 = CARTESIAN_POINT ( 'NONE',  ( -11.82391492285750090, 41.25980026458489647, -141.7018521871114558 ) ) ;
#9481 = FACE_OUTER_BOUND ( 'NONE', #22826, .T. ) ;
#9482 = DIRECTION ( 'NONE',  ( 2.256861364460000137E-12, 0.000000000000000000, 1.000000000000000000 ) ) ;
#9483 = ORIENTED_EDGE ( 'NONE', *, *, #6101, .F. ) ;
#9484 = DIRECTION ( 'NONE',  ( 0.1720749717299729364, 0.9850838563818457017, -6.484322019408987829E-13 ) ) ;
#9485 = DIRECTION ( 'NONE',  ( 1.000000000000000000, 0.000000000000000000, 0.000000000000000000 ) ) ;
#9486 = VECTOR ( 'NONE', #17543, 1000.000000000000227 ) ;
#9487 = AXIS2_PLACEMENT_3D ( 'NONE', #14565, #1365, #8592 ) ;
#9488 = EDGE_CURVE ( 'NONE', #915, #7205, #16690, .T. ) ;
#9489 = ORIENTED_EDGE ( 'NONE', *, *, #8203, .T. ) ;
#9490 = DIRECTION ( 'NONE',  ( 2.257749542879999954E-12, 0.000000000000000000, 1.000000000000000000 ) ) ;
#9491 = CARTESIAN_POINT ( 'NONE',  ( -27.87941100700000163, 36.27261185799999765, -147.6334388379999893 ) ) ;
#9492 = EDGE_LOOP ( 'NONE', ( #16476, #6769, #8336, #3357 ) ) ;
#9493 = VECTOR ( 'NONE', #15888, 1000.000000000000000 ) ;
#9494 = DIRECTION ( 'NONE',  ( 0.000000000000000000, 0.000000000000000000, -1.000000000000000000 ) ) ;
#9495 = CARTESIAN_POINT ( 'NONE',  ( -20.55139866887920164, 40.46905695053816743, -146.1780460796892100 ) ) ;
#9496 = EDGE_LOOP ( 'NONE', ( #10368, #2550, #9080, #13419, #21816 ) ) ;
#9497 = SURFACE_STYLE_FILL_AREA ( #22482 ) ;
#9498 = LINE ( 'NONE', #7486, #4242 ) ;
#9499 = CARTESIAN_POINT ( 'NONE',  ( 32.14594224169999848, -40.79958733389999992, -143.0552959529999839 ) ) ;
#9500 = ORIENTED_EDGE ( 'NONE', *, *, #18197, .F. ) ;
#9501 = CARTESIAN_POINT ( 'NONE',  ( 6.000000000140000012, 36.50000000000000000, -147.5552959529999839 ) ) ;
#9502 = CARTESIAN_POINT ( 'NONE',  ( -32.50000000000000000, 10.25000000000000000, -137.0552959530000123 ) ) ;
#9503 = ADVANCED_FACE ( 'NONE', ( #4662 ), #22983, .F. ) ;
#9504 = CARTESIAN_POINT ( 'NONE',  ( 2.170391987449999505, -12.72823260819999902, -145.5552959529999839 ) ) ;
#9505 = ORIENTED_EDGE ( 'NONE', *, *, #1853, .F. ) ;
#9506 = DIRECTION ( 'NONE',  ( -1.526468026909999897E-13, -8.159623473500000156E-13, -1.000000000000000000 ) ) ;
#9507 = CARTESIAN_POINT ( 'NONE',  ( -34.50000000000000000, 27.00000000000000000, -146.5552959529999839 ) ) ;
#9508 = ORIENTED_EDGE ( 'NONE', *, *, #11064, .F. ) ;
#9509 = AXIS2_PLACEMENT_3D ( 'NONE', #15102, #12842, #715 ) ;
#9510 = VECTOR ( 'NONE', #8245, 1000.000000000000114 ) ;
#9511 = EDGE_CURVE ( 'NONE', #4754, #20005, #15164, .T. ) ;
#9512 = EDGE_LOOP ( 'NONE', ( #21216, #17283, #14104, #18298 ) ) ;
#9513 = EDGE_CURVE ( 'NONE', #5292, #6470, #15605, .T. ) ;
#9514 = CARTESIAN_POINT ( 'NONE',  ( 2.139623390130000136, -12.81320239329999922, -144.0552959529999839 ) ) ;
#9515 = DIRECTION ( 'NONE',  ( 2.255973186040000320E-12, 0.000000000000000000, 1.000000000000000000 ) ) ;
#9516 = PRODUCT_DEFINITION_SHAPE ( 'NONE', 'NONE',  #10209 ) ;
#9517 = PLANE ( 'NONE',  #16608 ) ;
#9518 = CARTESIAN_POINT ( 'NONE',  ( 7.661531047501870084, 35.75622639781018108, -141.8866492539494857 ) ) ;
#9519 = ORIENTED_EDGE ( 'NONE', *, *, #8809, .T. ) ;
#9520 = DIRECTION ( 'NONE',  ( 1.526468026909999897E-13, 8.159623473500000156E-13, 1.000000000000000000 ) ) ;
#9521 = LINE ( 'NONE', #8202, #5532 ) ;
#9522 = EDGE_CURVE ( 'NONE', #2624, #2028, #23097, .T. ) ;
#9523 = CARTESIAN_POINT ( 'NONE',  ( -15.50000000000000000, 21.50000000000000000, -136.0552959530000123 ) ) ;
#9524 = DIRECTION ( 'NONE',  ( 1.000000000000000000, 2.602084704489999637E-17, 0.000000000000000000 ) ) ;
#9525 = CARTESIAN_POINT ( 'NONE',  ( -23.33899886291975889, 41.64279904421267986, -143.6714135781022605 ) ) ;
#9526 = EDGE_CURVE ( 'NONE', #14604, #17961, #21086, .T. ) ;
#9527 = VECTOR ( 'NONE', #12677, 1000.000000000000000 ) ;
#9528 = AXIS2_PLACEMENT_3D ( 'NONE', #2464, #14079, #2574 ) ;
#9529 = VECTOR ( 'NONE', #17762, 1000.000000000000114 ) ;
#9530 = CARTESIAN_POINT ( 'NONE',  ( -15.94523344361886075, 33.71216531385520199, -145.7766456663750034 ) ) ;
#9531 = EDGE_CURVE ( 'NONE', #21987, #7133, #15480, .T. ) ;
#9532 = EDGE_CURVE ( 'NONE', #2149, #4983, #12140, .T. ) ;
#9533 = PLANE ( 'NONE',  #4262 ) ;
#9534 = CARTESIAN_POINT ( 'NONE',  ( -2.499999999949999996, 34.00000000000000000, -150.0552959529999839 ) ) ;
#9535 = LINE ( 'NONE', #15016, #11155 ) ;
#9536 = ORIENTED_EDGE ( 'NONE', *, *, #881, .F. ) ;
#9537 = CARTESIAN_POINT ( 'NONE',  ( -6.882992773709530887, 38.62672044876698152, -147.5226783901907481 ) ) ;
#9538 = CARTESIAN_POINT ( 'NONE',  ( 1.342750202250000191, -63.28208324180000233, -144.5552959529999839 ) ) ;
#9539 = VERTEX_POINT ( 'NONE', #19415 ) ;
#9540 = CARTESIAN_POINT ( 'NONE',  ( -6.635402838469999232, -21.69968975860000171, -147.5552959529999839 ) ) ;
#9541 = CARTESIAN_POINT ( 'NONE',  ( -22.20363240416772399, 34.86754896295690997, -140.9631074518152332 ) ) ;
#9542 = VECTOR ( 'NONE', #11585, 1000.000000000000000 ) ;
#9543 = DIRECTION ( 'NONE',  ( -0.6459422414661291079, 0.7633862853691523176, -2.245315045000450442E-12 ) ) ;
#9544 = VERTEX_POINT ( 'NONE', #11901 ) ;
#9545 = CIRCLE ( 'NONE', #9158, 2.000000000000001776 ) ;
#9546 = CARTESIAN_POINT ( 'NONE',  ( -11.95558717921827885, 36.12952356042787727, -147.9535135442314129 ) ) ;
#9547 = DIRECTION ( 'NONE',  ( 0.000000000000000000, -1.000000000000000000, 0.000000000000000000 ) ) ;
#9548 = LINE ( 'NONE', #11207, #23451 ) ;
#9549 = CARTESIAN_POINT ( 'NONE',  ( 1.133692148550000001, 50.50000000000000000, -137.0552959530000123 ) ) ;
#9550 = CARTESIAN_POINT ( 'NONE',  ( 10.93320006080000084, -15.50000000000000000, -148.5552959529999839 ) ) ;
#9551 = DIRECTION ( 'NONE',  ( -3.994014904670000134E-29, 1.000000000000000000, 0.000000000000000000 ) ) ;
#9552 = EDGE_LOOP ( 'NONE', ( #20455, #10274, #5721, #6497 ) ) ;
#9553 = ADVANCED_FACE ( 'NONE', ( #19288 ), #10234, .F. ) ;
#9554 = CARTESIAN_POINT ( 'NONE',  ( -28.26195922703709229, 35.47171465400183621, -147.6105075849922059 ) ) ;
#9555 = ORIENTED_EDGE ( 'NONE', *, *, #3025, .T. ) ;
#9556 = VERTEX_POINT ( 'NONE', #12258 ) ;
#9557 = CARTESIAN_POINT ( 'NONE',  ( -14.19107797818078787, 33.22326183629838425, -142.1039242036714541 ) ) ;
#9558 = DIRECTION ( 'NONE',  ( 0.000000000000000000, -2.252420471819999940E-12, 1.000000000000000000 ) ) ;
#9559 = CIRCLE ( 'NONE', #6157, 1.500000000000001332 ) ;
#9560 = AXIS2_PLACEMENT_3D ( 'NONE', #17056, #22424, #12903 ) ;
#9561 = DIRECTION ( 'NONE',  ( 0.000000000000000000, 0.000000000000000000, 1.000000000000000000 ) ) ;
#9562 = CIRCLE ( 'NONE', #12613, 2.000000000000000000 ) ;
#9563 = ORIENTED_EDGE ( 'NONE', *, *, #13997, .T. ) ;
#9564 = DIRECTION ( 'NONE',  ( -1.000000000000000000, 0.000000000000000000, 0.000000000000000000 ) ) ;
#9565 = LINE ( 'NONE', #13140, #3810 ) ;
#9566 = VERTEX_POINT ( 'NONE', #19533 ) ;
#9567 = CARTESIAN_POINT ( 'NONE',  ( -20.40768304764253216, 38.39967751248821770, -140.8966145518345456 ) ) ;
#9568 = CARTESIAN_POINT ( 'NONE',  ( 9.246789369175132833, 38.30178617907670002, -141.9207453424001528 ) ) ;
#9569 = CARTESIAN_POINT ( 'NONE',  ( -32.50000000000000000, -1.000000000000000000, -151.0552959529999839 ) ) ;
#9570 = CARTESIAN_POINT ( 'NONE',  ( -28.06178240310348571, 37.06443177824644408, -147.7991814974818396 ) ) ;
#9571 = ORIENTED_EDGE ( 'NONE', *, *, #1847, .F. ) ;
#9572 = VECTOR ( 'NONE', #12341, 1000.000000000000114 ) ;
#9573 = ADVANCED_FACE ( 'NONE', ( #3227 ), #7267, .T. ) ;
#9574 = LINE ( 'NONE', #10264, #8411 ) ;
#9575 = ORIENTED_EDGE ( 'NONE', *, *, #22935, .T. ) ;
#9576 = CARTESIAN_POINT ( 'NONE',  ( 8.100000000049998761, 37.00000000000000000, -149.5552959529999839 ) ) ;
#9577 = ORIENTED_EDGE ( 'NONE', *, *, #16106, .T. ) ;
#9578 = CARTESIAN_POINT ( 'NONE',  ( 13.13369214859999978, -51.50000000000000000, -137.0552959530000123 ) ) ;
#9579 = ORIENTED_EDGE ( 'NONE', *, *, #22249, .T. ) ;
#9580 = CARTESIAN_POINT ( 'NONE',  ( -22.18841299866283379, 32.72156082663942556, -146.4695531048793953 ) ) ;
#9581 = EDGE_LOOP ( 'NONE', ( #9625, #18870, #15666, #3940 ) ) ;
#9582 = DIRECTION ( 'NONE',  ( 1.000000000000000000, 0.000000000000000000, 0.000000000000000000 ) ) ;
#9583 = ORIENTED_EDGE ( 'NONE', *, *, #7340, .F. ) ;
#9584 = DIRECTION ( 'NONE',  ( 0.000000000000000000, 0.000000000000000000, 1.000000000000000000 ) ) ;
#9585 = EDGE_LOOP ( 'NONE', ( #19606, #12689, #10995, #10903 ) ) ;
#9586 = FACE_OUTER_BOUND ( 'NONE', #5827, .T. ) ;
#9587 = CARTESIAN_POINT ( 'NONE',  ( -14.31404048459999956, 38.45176613019999934, -140.7319883510000125 ) ) ;
#9588 = CARTESIAN_POINT ( 'NONE',  ( 8.446000075252877437, 27.76013181716563594, -150.0552959529999555 ) ) ;
#9589 = MECHANICAL_DESIGN_GEOMETRIC_PRESENTATION_REPRESENTATION (  '', ( #20269 ), #5814 ) ;
#9590 = AXIS2_PLACEMENT_3D ( 'NONE', #6793, #3591, #5599 ) ;
#9591 = DIRECTION ( 'NONE',  ( 1.000000000000000000, 0.000000000000000000, 0.000000000000000000 ) ) ;
#9592 = CARTESIAN_POINT ( 'NONE',  ( -9.005502668621559792, 40.51905748780640693, -141.9284054814384035 ) ) ;
#9593 = VERTEX_POINT ( 'NONE', #3584 ) ;
#9594 = CARTESIAN_POINT ( 'NONE',  ( 32.50000000000000000, 39.80430157320000006, -149.8052959529999839 ) ) ;
#9595 = B_SPLINE_CURVE_WITH_KNOTS ( 'NONE', 5,
 ( #21247, #4940, #5163, #1625, #12187, #3164, #3268, #10394, #1376, #8603, #10501, #12412 ),
 .UNSPECIFIED., .F., .F.,
 ( 6, 3, 3, 6 ),
 ( 0.000000000000000000, 4.358589029760000066, 8.533830367689999363, 12.54112731390000057 ),
 .UNSPECIFIED. ) ;
#9596 = DIRECTION ( 'NONE',  ( 2.507554887169999917E-12, 0.000000000000000000, -1.000000000000000000 ) ) ;
#9597 = DIRECTION ( 'NONE',  ( -0.7432941462487078210, 0.000000000000000000, -0.6689647316207368855 ) ) ;
#9598 = EDGE_LOOP ( 'NONE', ( #12233, #1008, #5665, #21862 ) ) ;
#9599 = CARTESIAN_POINT ( 'NONE',  ( -11.80427317207966098, 41.71109129671971516, -144.7115759666664303 ) ) ;
#9600 = ADVANCED_FACE ( 'NONE', ( #2048 ), #10812, .F. ) ;
#9601 = CARTESIAN_POINT ( 'NONE',  ( -18.28762386024642339, 39.85118522382028772, -147.8656472858100983 ) ) ;
#9602 = CARTESIAN_POINT ( 'NONE',  ( -29.95441468910000182, 40.29796007080000209, -145.3430615500000158 ) ) ;
#9603 = ORIENTED_EDGE ( 'NONE', *, *, #497, .F. ) ;
#9604 = LINE ( 'NONE', #2147, #22328 ) ;
#9605 = EDGE_CURVE ( 'NONE', #11959, #8849, #7024, .T. ) ;
#9606 = CARTESIAN_POINT ( 'NONE',  ( 9.152949117179998595, -16.59780702190000312, -148.5552959529999839 ) ) ;
#9607 = VERTEX_POINT ( 'NONE', #16540 ) ;
#9608 = CYLINDRICAL_SURFACE ( 'NONE', #6920, 0.7500000000000006661 ) ;
#9609 = ORIENTED_EDGE ( 'NONE', *, *, #21131, .F. ) ;
#9610 = FACE_OUTER_BOUND ( 'NONE', #17472, .T. ) ;
#9611 = CARTESIAN_POINT ( 'NONE',  ( -21.73552493300723754, 38.87455327618756940, -148.2354957168025180 ) ) ;
#9612 = ORIENTED_EDGE ( 'NONE', *, *, #8853, .T. ) ;
#9613 =( BOUNDED_SURFACE ( )  B_SPLINE_SURFACE ( 5, 5, ( 
 ( #15040, #22301, #5992, #10377, #20996, #17295 ),
 ( #15635, #14087, #6699, #1481, #8704, #12173 ),
 ( #13730, #4806, #15985, #15750, #8589, #23012 ),
 ( #17413, #23247, #14204, #10020, #6940, #2792 ),
 ( #4690, #3147, #8239, #15860, #21355, #21466 ),
 ( #19086, #1136, #1011, #19448, #10271, #11930 ),
 ( #5045, #19319, #22771, #5146, #19560, #17537 ),
 ( #15512, #6471, #21230, #8366, #2907, #23126 ),
 ( #17766, #19195, #10139, #4926, #13849, #1255 ),
 ( #17654, #13961, #22900, #1360, #6584, #21114 ),
 ( #12049, #3033, #6818, #12287, #3253, #8482 ),
 ( #10487, #14314, #14786, #48, #12642, #21586 ) ),
 .UNSPECIFIED., .F., .F., .F. ) 
 B_SPLINE_SURFACE_WITH_KNOTS ( ( 6, 3, 3, 6 ),
 ( 6, 6 ),
 ( 0.000000000000000000, 4.346865784160000246, 8.778337911509998648, 13.29702284770000098 ),
 ( 0.000000000000000000, 1.570796326891464867 ),
 .UNSPECIFIED. ) 
 GEOMETRIC_REPRESENTATION_ITEM ( )  RATIONAL_B_SPLINE_SURFACE ( (
 ( 1.000000000000000000, 0.5999999999754349611, 0.3999999999754355051, 0.2999999999815765039, 0.2499999999877174917, 0.2500000000000000000),
 ( 1.000000000000000000, 0.5999999999754349611, 0.3999999999754355051, 0.2999999999815765039, 0.2499999999877174917, 0.2500000000000000000),
 ( 1.000000000000000000, 0.5999999999754349611, 0.3999999999754355051, 0.2999999999815765039, 0.2499999999877174917, 0.2500000000000000000),
 ( 1.000000000000000000, 0.5999999999754349611, 0.3999999999754355051, 0.2999999999815765039, 0.2499999999877174917, 0.2500000000000000000),
 ( 1.000000000000000000, 0.5999999999754349611, 0.3999999999754355051, 0.2999999999815765039, 0.2499999999877174917, 0.2500000000000000000),
 ( 1.000000000000000000, 0.5999999999754349611, 0.3999999999754355051, 0.2999999999815765039, 0.2499999999877174917, 0.2500000000000000000),
 ( 1.000000000000000000, 0.5999999999754349611, 0.3999999999754355051, 0.2999999999815765039, 0.2499999999877174917, 0.2500000000000000000),
 ( 1.000000000000000000, 0.5999999999754349611, 0.3999999999754355051, 0.2999999999815765039, 0.2499999999877174917, 0.2500000000000000000),
 ( 1.000000000000000000, 0.5999999999754349611, 0.3999999999754355051, 0.2999999999815765039, 0.2499999999877174917, 0.2500000000000000000),
 ( 1.000000000000000000, 0.5999999999754349611, 0.3999999999754355051, 0.2999999999815765039, 0.2499999999877174917, 0.2500000000000000000),
 ( 1.000000000000000000, 0.5999999999754349611, 0.3999999999754355051, 0.2999999999815765039, 0.2499999999877174917, 0.2500000000000000000),
 ( 1.000000000000000000, 0.5999999999754349611, 0.3999999999754355051, 0.2999999999815765039, 0.2499999999877174917, 0.2500000000000000000) ) ) 
 REPRESENTATION_ITEM ( '' )  SURFACE ( )  );
#9614 = CARTESIAN_POINT ( 'NONE',  ( -28.07061429630000049, 34.82490105569999628, -147.0351741510000068 ) ) ;
#9615 = FACE_OUTER_BOUND ( 'NONE', #19384, .T. ) ;
#9616 = ORIENTED_EDGE ( 'NONE', *, *, #12301, .F. ) ;
#9617 = DIRECTION ( 'NONE',  ( 0.000000000000000000, -1.000000000000000000, 0.000000000000000000 ) ) ;
#9618 = LINE ( 'NONE', #6068, #14132 ) ;
#9619 = CARTESIAN_POINT ( 'NONE',  ( -21.55459145674873866, -4.749999999999015010, -146.3157682190004891 ) ) ;
#9620 = ORIENTED_EDGE ( 'NONE', *, *, #18884, .T. ) ;
#9621 = CARTESIAN_POINT ( 'NONE',  ( 10.94417203217891021, -19.52598336879741936, -148.5552959530000123 ) ) ;
#9622 = CARTESIAN_POINT ( 'NONE',  ( -15.19886026855731842, -44.49999999999996447, -136.0552959529656789 ) ) ;
#9623 = ORIENTED_EDGE ( 'NONE', *, *, #15028, .T. ) ;
#9624 = ADVANCED_FACE ( 'NONE', ( #21799 ), #14288, .F. ) ;
#9625 = ORIENTED_EDGE ( 'NONE', *, *, #9306, .F. ) ;
#9626 = CYLINDRICAL_SURFACE ( 'NONE', #8588, 0.7500000000000006661 ) ;
#9627 = PLANE ( 'NONE',  #6650 ) ;
#9628 = DIRECTION ( 'NONE',  ( 2.257144641399999941E-12, 0.000000000000000000, 1.000000000000000000 ) ) ;
#9629 = CARTESIAN_POINT ( 'NONE',  ( 23.19105773460000108, -15.44374190390000123, -145.5552959529999839 ) ) ;
#9630 = ORIENTED_EDGE ( 'NONE', *, *, #99, .T. ) ;
#9631 = DIRECTION ( 'NONE',  ( 0.000000000000000000, -1.000000000000000000, 8.159623473500000156E-13 ) ) ;
#9632 = EDGE_CURVE ( 'NONE', #6404, #12670, #19770, .T. ) ;
#9633 = LINE ( 'NONE', #864, #227 ) ;
#9634 = CARTESIAN_POINT ( 'NONE',  ( -14.60945070276051894, -41.53817725281877671, -150.0552959529999839 ) ) ;
#9635 = CARTESIAN_POINT ( 'NONE',  ( 22.50000000000000000, 33.50000000000000000, -151.0552959529999839 ) ) ;
#9636 = DIRECTION ( 'NONE',  ( 1.000000000000000000, 0.000000000000000000, 0.000000000000000000 ) ) ;
#9637 = DIRECTION ( 'NONE',  ( 0.000000000000000000, 0.000000000000000000, 1.000000000000000000 ) ) ;
#9638 = VECTOR ( 'NONE', #19562, 1000.000000000000000 ) ;
#9639 = CARTESIAN_POINT ( 'NONE',  ( -17.55745234320254866, 36.93608508457231920, -140.4812394865591045 ) ) ;
#9640 = EDGE_CURVE ( 'NONE', #11584, #12574, #1694, .T. ) ;
#9641 = CARTESIAN_POINT ( 'NONE',  ( -7.816799939239999162, -0.2500000000010000334, -148.5552959529999839 ) ) ;
#9642 = CARTESIAN_POINT ( 'NONE',  ( 6.500000000000000000, 13.00000000000000000, -151.0552959529999839 ) ) ;
#9643 = DIRECTION ( 'NONE',  ( -1.525446435830000185E-13, -8.171241461240000022E-13, -1.000000000000000000 ) ) ;
#9644 = ORIENTED_EDGE ( 'NONE', *, *, #15213, .T. ) ;
#9645 = CARTESIAN_POINT ( 'NONE',  ( -5.251527070960000820, 40.93408815870000694, -143.6492421949999994 ) ) ;
#9646 = FACE_BOUND ( 'NONE', #4399, .T. ) ;
#9647 = ORIENTED_EDGE ( 'NONE', *, *, #11511, .F. ) ;
#9648 = DIRECTION ( 'NONE',  ( 0.000000000000000000, -2.252420472359999842E-12, -1.000000000000000000 ) ) ;
#9649 = ADVANCED_FACE ( 'NONE', ( #12616, #23334 ), #9152, .T. ) ;
#9650 = EDGE_CURVE ( 'NONE', #15634, #10783, #12487, .T. ) ;
#9651 = CARTESIAN_POINT ( 'NONE',  ( -22.31464002779999944, 34.51618902799999944, -147.4864127260000259 ) ) ;
#9652 = DIRECTION ( 'NONE',  ( 1.000000000000000000, 0.000000000000000000, -2.259525899719999991E-12 ) ) ;
#9653 = ORIENTED_EDGE ( 'NONE', *, *, #14495, .F. ) ;
#9654 = CARTESIAN_POINT ( 'NONE',  ( -12.28742291280838650, 34.42299388273512761, -147.6510490011623631 ) ) ;
#9655 = ADVANCED_FACE ( 'NONE', ( #14643 ), #11056, .F. ) ;
#9656 = DIRECTION ( 'NONE',  ( 5.094701932209999624E-24, 1.000000000000000000, 0.000000000000000000 ) ) ;
#9657 = EDGE_CURVE ( 'NONE', #4528, #12438, #1319, .T. ) ;
#9658 = CARTESIAN_POINT ( 'NONE',  ( 24.89581725840000104, -26.85672394480000236, -143.5552959529999839 ) ) ;
#9659 = CARTESIAN_POINT ( 'NONE',  ( -27.77832206610000298, 37.03059619289999915, -147.6270870419999710 ) ) ;
#9660 = CARTESIAN_POINT ( 'NONE',  ( 12.68320006080000084, -24.50000000000000000, -149.3052959529999839 ) ) ;
#9661 = LINE ( 'NONE', #21954, #6366 ) ;
#9662 = EDGE_LOOP ( 'NONE', ( #2011, #16586, #15484, #16108 ) ) ;
#9663 = CARTESIAN_POINT ( 'NONE',  ( -27.87941100700000163, 36.27261185799999765, -147.6334388379999893 ) ) ;
#9664 = VERTEX_POINT ( 'NONE', #18906 ) ;
#9665 = EDGE_CURVE ( 'NONE', #12941, #11596, #16890, .T. ) ;
#9666 = CARTESIAN_POINT ( 'NONE',  ( -13.02237250279999969, 32.42872598539999274, -144.6889042450000034 ) ) ;
#9667 = CARTESIAN_POINT ( 'NONE',  ( -10.65913935279999869, 37.04331329920000115, -139.7140392919999954 ) ) ;
#9668 = LINE ( 'NONE', #4571, #16501 ) ;
#9669 = ADVANCED_FACE ( 'NONE', ( #4049 ), #15344, .F. ) ;
#9670 = EDGE_LOOP ( 'NONE', ( #17205, #7345, #1722, #6331 ) ) ;
#9671 = CARTESIAN_POINT ( 'NONE',  ( 31.50000000000000000, 32.96379895120000469, -137.0552959530000123 ) ) ;
#9672 = FACE_OUTER_BOUND ( 'NONE', #22648, .T. ) ;
#9673 = VECTOR ( 'NONE', #19402, 1000.000000000000000 ) ;
#9674 = VERTEX_POINT ( 'NONE', #7835 ) ;
#9675 = CARTESIAN_POINT ( 'NONE',  ( -20.49955794677946130, 40.53802795458025088, -144.5257500491008500 ) ) ;
#9676 = ADVANCED_FACE ( 'NONE', ( #15104, #6290, #20816 ), #17125, .F. ) ;
#9677 = VECTOR ( 'NONE', #22684, 1000.000000000000000 ) ;
#9678 = CARTESIAN_POINT ( 'NONE',  ( 9.342139795696894566, 38.24129265476425843, -141.8852171080566507 ) ) ;
#9679 = EDGE_CURVE ( 'NONE', #12200, #12791, #22387, .T. ) ;
#9680 = CARTESIAN_POINT ( 'NONE',  ( 7.512097219667818848, 35.86684335154615155, -146.2851006690084148 ) ) ;
#9681 = CARTESIAN_POINT ( 'NONE',  ( -22.52780672249999938, 37.05898997719999954, -140.0074087190000114 ) ) ;
#9682 = CARTESIAN_POINT ( 'NONE',  ( 25.15155135439999867, -26.08415009650000016, -147.5552959529999839 ) ) ;
#9683 = ORIENTED_EDGE ( 'NONE', *, *, #11345, .T. ) ;
#9684 = CARTESIAN_POINT ( 'NONE',  ( -6.635402838459999231, -21.69968975860000171, -146.5552959529999839 ) ) ;
#9685 = ORIENTED_EDGE ( 'NONE', *, *, #11125, .T. ) ;
#9686 = AXIS2_PLACEMENT_3D ( 'NONE', #16933, #7877, #11563 ) ;
#9687 = CARTESIAN_POINT ( 'NONE',  ( -4.500000000000000000, 34.00000000000000000, -150.0552959529999839 ) ) ;
#9688 = EDGE_LOOP ( 'NONE', ( #13278, #7353 ) ) ;
#9689 = CARTESIAN_POINT ( 'NONE',  ( -27.67795712710000089, 37.78351609900000341, -147.6208067679999942 ) ) ;
#9690 = ORIENTED_EDGE ( 'NONE', *, *, #21374, .T. ) ;
#9691 = CARTESIAN_POINT ( 'NONE',  ( -22.82643395159999855, 32.86988923359999859, -143.6006525860000238 ) ) ;
#9692 = VERTEX_POINT ( 'NONE', #13544 ) ;
#9693 = CARTESIAN_POINT ( 'NONE',  ( -14.60730091830126476, -46.00000000000000711, -150.0552959529999555 ) ) ;
#9694 = ORIENTED_EDGE ( 'NONE', *, *, #4374, .F. ) ;
#9695 = EDGE_LOOP ( 'NONE', ( #13320, #11951, #14954, #22566 ) ) ;
#9696 = DIRECTION ( 'NONE',  ( 0.9988198443106121038, -0.04856869991388110958, -1.110673412899570175E-14 ) ) ;
#9697 = CARTESIAN_POINT ( 'NONE',  ( 4.999999999879999990, -4.000000000000000000, -135.4552959529999896 ) ) ;
#9698 = DIRECTION ( 'NONE',  ( 0.2024296638729825848, 0.9792968044389154247, -3.587490878269691778E-13 ) ) ;
#9699 = LINE ( 'NONE', #13058, #17808 ) ;
#9700 = DIRECTION ( 'NONE',  ( 0.000000000000000000, -1.000000000000000000, 0.000000000000000000 ) ) ;
#9701 = EDGE_CURVE ( 'NONE', #2580, #4564, #18443, .T. ) ;
#9702 = CARTESIAN_POINT ( 'NONE',  ( -8.613431449137619822, 37.75849558873363776, -140.1079839314714093 ) ) ;
#9703 = ORIENTED_EDGE ( 'NONE', *, *, #22924, .F. ) ;
#9704 = DIRECTION ( 'NONE',  ( -2.507771768019999718E-12, -1.592654864069999939E-17, 1.000000000000000000 ) ) ;
#9705 = AXIS2_PLACEMENT_3D ( 'NONE', #18326, #10801, #5359 ) ;
#9706 = CARTESIAN_POINT ( 'NONE',  ( 9.252789717580752082, 38.29861131861105150, -146.1917200022118948 ) ) ;
#9707 = LINE ( 'NONE', #6042, #9442 ) ;
#9708 = ORIENTED_EDGE ( 'NONE', *, *, #14375, .T. ) ;
#9709 = CARTESIAN_POINT ( 'NONE',  ( -12.30631862527572018, 40.23402543372416318, -145.9987124283284174 ) ) ;
#9710 = CARTESIAN_POINT ( 'NONE',  ( 1.133692148550000001, 51.50000000000000000, -136.0552959530000123 ) ) ;
#9711 = CARTESIAN_POINT ( 'NONE',  ( 10.68320006080000084, -19.50000000000000000, -148.5552959529999839 ) ) ;
#9712 = ORIENTED_EDGE ( 'NONE', *, *, #23330, .T. ) ;
#9713 = CARTESIAN_POINT ( 'NONE',  ( -32.50000000000000000, 28.00000000000000000, -141.5552959529999839 ) ) ;
#9714 = LINE ( 'NONE', #16991, #17713 ) ;
#9715 = ORIENTED_EDGE ( 'NONE', *, *, #8148, .F. ) ;
#9716 = DIRECTION ( 'NONE',  ( -0.09606172499277226828, -0.9953753789357124848, 8.268372250837614805E-13 ) ) ;
#9717 = CARTESIAN_POINT ( 'NONE',  ( -25.35824191590000254, -18.00000000000000000, -144.8157682190000060 ) ) ;
#9718 = ORIENTED_EDGE ( 'NONE', *, *, #1721, .T. ) ;
#9719 = DIRECTION ( 'NONE',  ( 1.526468026909999897E-13, 8.159623473500000156E-13, 1.000000000000000000 ) ) ;
#9720 = VECTOR ( 'NONE', #10855, 1000.000000000000000 ) ;
#9721 = CARTESIAN_POINT ( 'NONE',  ( -19.69393976299120297, 37.84845892289124691, -140.3168504268994070 ) ) ;
#9722 = VERTEX_POINT ( 'NONE', #9501 ) ;
#9723 =( NAMED_UNIT ( * ) PLANE_ANGLE_UNIT ( ) SI_UNIT ( $, .RADIAN. ) );
#9724 = CARTESIAN_POINT ( 'NONE',  ( -27.36101731545187477, 33.42236680594814402, -145.9827244586238919 ) ) ;
#9725 = DIRECTION ( 'NONE',  ( 2.842170943040000002E-14, 3.552713678800000097E-13, 1.000000000000000000 ) ) ;
#9726 = ORIENTED_EDGE ( 'NONE', *, *, #19590, .T. ) ;
#9727 = CARTESIAN_POINT ( 'NONE',  ( 6.500000000030000002, 20.50000000000000000, -137.0552959530000123 ) ) ;
#9728 = CARTESIAN_POINT ( 'NONE',  ( -4.499999999929999994, 40.00000000000000000, -138.0552959530000123 ) ) ;
#9729 = CARTESIAN_POINT ( 'NONE',  ( 24.09267687515769296, -30.62512331353721251, -146.5552959530036503 ) ) ;
#9730 = ORIENTED_EDGE ( 'NONE', *, *, #11688, .T. ) ;
#9731 = EDGE_CURVE ( 'NONE', #3632, #16983, #18557, .T. ) ;
#9732 = CARTESIAN_POINT ( 'NONE',  ( 10.68320006080000084, -19.50000000000000000, -148.5552959529999839 ) ) ;
#9733 = CARTESIAN_POINT ( 'NONE',  ( 15.97954986339999905, -26.72957102550000030, -143.5552959529999839 ) ) ;
#9734 = EDGE_CURVE ( 'NONE', #21227, #8089, #11630, .T. ) ;
#9735 = ORIENTED_EDGE ( 'NONE', *, *, #19791, .F. ) ;
#9736 = VECTOR ( 'NONE', #3920, 999.9999999999998863 ) ;
#9737 = ORIENTED_EDGE ( 'NONE', *, *, #2558, .F. ) ;
#9738 = CARTESIAN_POINT ( 'NONE',  ( 16.13369214829999976, -51.50000000000000000, -136.0552959530000123 ) ) ;
#9739 = DIRECTION ( 'NONE',  ( 1.000000000000000000, 0.000000000000000000, -2.257120985840000117E-12 ) ) ;
#9740 = CARTESIAN_POINT ( 'NONE',  ( -10.00000000000000000, 19.50000000000000000, -150.0552959529999839 ) ) ;
#9741 = CARTESIAN_POINT ( 'NONE',  ( -9.347107914279998653, -17.32706600430000066, -143.5552959529999839 ) ) ;
#9742 = ORIENTED_EDGE ( 'NONE', *, *, #11668, .F. ) ;
#9743 = DIRECTION ( 'NONE',  ( -1.000000000000000000, 0.000000000000000000, -2.273736754430000208E-12 ) ) ;
#9744 = DIRECTION ( 'NONE',  ( 0.9991304227374304681, 0.04169410462551791791, -4.019436694231727866E-14 ) ) ;
#9745 =( BOUNDED_CURVE ( )  B_SPLINE_CURVE ( 5, ( #8153, #11722, #13404, #12084, #10176, #6265 ),
 .UNSPECIFIED., .F., .F. ) 
 B_SPLINE_CURVE_WITH_KNOTS ( ( 6, 6 ),
 ( 0.000000000000000000, 1.570796326630344186 ),
 .UNSPECIFIED. ) 
 CURVE ( )  GEOMETRIC_REPRESENTATION_ITEM ( )  RATIONAL_B_SPLINE_CURVE ( ( 1.000000000000000000, 0.6000000000419293267, 0.4000000000419293156, 0.3000000000314470006, 0.2500000000209646744, 0.2500000000000000555 ) ) 
 REPRESENTATION_ITEM ( '' )  );
#9746 = CARTESIAN_POINT ( 'NONE',  ( 0.000000000000000000, 0.000000000000000000, -150.0552959529999839 ) ) ;
#9747 = CARTESIAN_POINT ( 'NONE',  ( -32.50000000000000000, 48.00000000000000000, -146.5552959529999839 ) ) ;
#9748 = CARTESIAN_POINT ( 'NONE',  ( 14.00000000000000000, 20.50000000000000000, -136.5552959530000123 ) ) ;
#9749 = CARTESIAN_POINT ( 'NONE',  ( -15.47773836757839661, 32.88821176121729195, -146.1526184873809200 ) ) ;
#9750 = VECTOR ( 'NONE', #5061, 1000.000000000000000 ) ;
#9751 = CARTESIAN_POINT ( 'NONE',  ( -14.47770030809999930, -34.50000000000000000, -147.5552959529999839 ) ) ;
#9752 = AXIS2_PLACEMENT_3D ( 'NONE', #14923, #22180, #11562 ) ;
#9753 = DIRECTION ( 'NONE',  ( 0.9949850929136110356, -0.1000233216789610247, 7.446425804567098138E-15 ) ) ;
#9754 = CARTESIAN_POINT ( 'NONE',  ( 6.000000000010000001, -3.500000000000000000, -136.0552959530000123 ) ) ;
#9755 = LINE ( 'NONE', #1230, #23339 ) ;
#9756 = ORIENTED_EDGE ( 'NONE', *, *, #20450, .F. ) ;
#9757 = CARTESIAN_POINT ( 'NONE',  ( -10.47418533556643894, 33.50012463686687880, -145.9259304112847815 ) ) ;
#9758 = DIRECTION ( 'NONE',  ( -1.000000000000000000, 0.000000000000000000, 0.000000000000000000 ) ) ;
#9759 = EDGE_CURVE ( 'NONE', #2337, #5226, #490, .T. ) ;
#9760 = ORIENTED_EDGE ( 'NONE', *, *, #16317, .F. ) ;
#9761 = CARTESIAN_POINT ( 'NONE',  ( 0.1832000607640000001, -3.000000000000000000, -148.5552959529999839 ) ) ;
#9762 = CARTESIAN_POINT ( 'NONE',  ( -21.83347610788520043, 32.92361448635804066, -143.4947777357014047 ) ) ;
#9763 = CARTESIAN_POINT ( 'NONE',  ( 7.750000000000000000, -41.23606797749999942, -150.0552959529999839 ) ) ;
#9764 = ORIENTED_EDGE ( 'NONE', *, *, #17234, .T. ) ;
#9765 = CARTESIAN_POINT ( 'NONE',  ( -12.60451255900682277, 35.62527299504891687, -147.2474940801387788 ) ) ;
#9766 = AXIS2_PLACEMENT_3D ( 'NONE', #18806, #9628, #16902 ) ;
#9767 = LINE ( 'NONE', #530, #2909 ) ;
#9768 = EDGE_CURVE ( 'NONE', #17827, #6145, #22599, .T. ) ;
#9769 = AXIS2_PLACEMENT_3D ( 'NONE', #15712, #6426, #2637 ) ;
#9770 = DIRECTION ( 'NONE',  ( 1.000000000000000000, 0.000000000000000000, 0.000000000000000000 ) ) ;
#9771 = DIRECTION ( 'NONE',  ( 0.000000000000000000, 0.000000000000000000, -1.000000000000000000 ) ) ;
#9772 = DIRECTION ( 'NONE',  ( -0.09606172499277226828, -0.9953753789357124848, 8.268372250837614805E-13 ) ) ;
#9773 = CARTESIAN_POINT ( 'NONE',  ( 7.930443943682751851, -33.22545875219810796, -150.0552959529999839 ) ) ;
#9774 = ORIENTED_EDGE ( 'NONE', *, *, #11692, .F. ) ;
#9775 = FACE_BOUND ( 'NONE', #13425, .T. ) ;
#9776 =( NAMED_UNIT ( * ) SI_UNIT ( $, .STERADIAN. ) SOLID_ANGLE_UNIT ( ) );
#9777 = EDGE_CURVE ( 'NONE', #16462, #22505, #9377, .T. ) ;
#9778 = ORIENTED_EDGE ( 'NONE', *, *, #14834, .F. ) ;
#9779 = CARTESIAN_POINT ( 'NONE',  ( -13.57921699037008523, 33.70180771155908417, -146.1646008835299995 ) ) ;
#9780 = LINE ( 'NONE', #13134, #19844 ) ;
#9781 = CARTESIAN_POINT ( 'NONE',  ( -11.14725012360000100, -1.500000000000000000, -148.5552959529999839 ) ) ;
#9782 = EDGE_CURVE ( 'NONE', #565, #20697, #14989, .T. ) ;
#9783 = CIRCLE ( 'NONE', #15123, 0.7500000000000006661 ) ;
#9784 = ORIENTED_EDGE ( 'NONE', *, *, #377, .T. ) ;
#9785 = DIRECTION ( 'NONE',  ( 0.000000000000000000, 0.000000000000000000, 1.000000000000000000 ) ) ;
#9786 = CARTESIAN_POINT ( 'NONE',  ( -14.47770030809999930, -1.500000000000000000, -147.5552959529999839 ) ) ;
#9787 = AXIS2_PLACEMENT_3D ( 'NONE', #2926, #2808, #1159 ) ;
#9788 = ORIENTED_EDGE ( 'NONE', *, *, #17660, .F. ) ;
#9789 = FACE_OUTER_BOUND ( 'NONE', #22742, .T. ) ;
#9790 = CARTESIAN_POINT ( 'NONE',  ( -18.61313235484081829, 39.16608643220034480, -146.8838699807833450 ) ) ;
#9791 = CARTESIAN_POINT ( 'NONE',  ( 7.706401777573996803, 35.72582932411368262, -146.2064413145237154 ) ) ;
#9792 = DIRECTION ( 'NONE',  ( -1.701177084980000217E-20, -4.426606872460000157E-37, -1.000000000000000000 ) ) ;
#9793 = ADVANCED_FACE ( 'NONE', ( #13082 ), #13317, .F. ) ;
#9794 = CARTESIAN_POINT ( 'NONE',  ( -25.73504040789999792, 33.16200571349999393, -143.7184748760000161 ) ) ;
#9795 = VERTEX_POINT ( 'NONE', #13195 ) ;
#9796 = EDGE_CURVE ( 'NONE', #21283, #18104, #10208, .T. ) ;
#9797 = AXIS2_PLACEMENT_3D ( 'NONE', #20302, #3992, #22522 ) ;
#9798 = AXIS2_PLACEMENT_3D ( 'NONE', #11033, #5682, #11145 ) ;
#9799 = LINE ( 'NONE', #20540, #19052 ) ;
#9800 = AXIS2_PLACEMENT_3D ( 'NONE', #16006, #11079, #1277 ) ;
#9801 = ORIENTED_EDGE ( 'NONE', *, *, #9526, .F. ) ;
#9802 = CARTESIAN_POINT ( 'NONE',  ( 15.87827223000000032, -26.60524292859999917, -144.0552959529999839 ) ) ;
#9803 = ORIENTED_EDGE ( 'NONE', *, *, #19864, .F. ) ;
#9804 = EDGE_CURVE ( 'NONE', #9978, #7971, #7724, .T. ) ;
#9805 = ORIENTED_EDGE ( 'NONE', *, *, #12624, .F. ) ;
#9806 = VECTOR ( 'NONE', #4871, 1000.000000000000000 ) ;
#9807 = LINE ( 'NONE', #17201, #17053 ) ;
#9808 = EDGE_CURVE ( 'NONE', #6526, #13263, #7953, .T. ) ;
#9809 = EDGE_LOOP ( 'NONE', ( #6260, #22002, #17630, #9293 ) ) ;
#9810 = CARTESIAN_POINT ( 'NONE',  ( -4.499999999959999109, 40.00000000000000000, -151.5552959529999839 ) ) ;
#9811 = ORIENTED_EDGE ( 'NONE', *, *, #12973, .T. ) ;
#9812 = EDGE_CURVE ( 'NONE', #14599, #5119, #20488, .T. ) ;
#9813 = ORIENTED_EDGE ( 'NONE', *, *, #16514, .T. ) ;
#9814 = CARTESIAN_POINT ( 'NONE',  ( -28.18164916501774897, 37.07873981899407312, -148.1638686016682414 ) ) ;
#9815 = CARTESIAN_POINT ( 'NONE',  ( -46.50000000000000000, 26.50000000000000000, -149.0552959529999839 ) ) ;
#9816 = CARTESIAN_POINT ( 'NONE',  ( -10.71787290739701781, 39.39257728183631002, -141.0168776336601582 ) ) ;
#9817 =( NAMED_UNIT ( * ) SI_UNIT ( $, .STERADIAN. ) SOLID_ANGLE_UNIT ( ) );
#9818 = CARTESIAN_POINT ( 'NONE',  ( -34.50000000000000000, -1.000000000000000000, -140.0552959529999839 ) ) ;
#9819 = AXIS2_PLACEMENT_3D ( 'NONE', #3678, #8895, #21537 ) ;
#9820 = CARTESIAN_POINT ( 'NONE',  ( -8.664978901450041349, 37.83471353584230457, -139.7100943505009809 ) ) ;
#9821 = ORIENTED_EDGE ( 'NONE', *, *, #21131, .T. ) ;
#9822 = AXIS2_PLACEMENT_3D ( 'NONE', #20546, #803, #22675 ) ;
#9823 = LINE ( 'NONE', #2372, #10585 ) ;
#9824 = VECTOR ( 'NONE', #12490, 1000.000000000000000 ) ;
#9825 = DIRECTION ( 'NONE',  ( -1.377713942929999840E-10, 1.000000000000000000, 0.000000000000000000 ) ) ;
#9826 = AXIS2_PLACEMENT_3D ( 'NONE', #15209, #1049, #18885 ) ;
#9827 = CARTESIAN_POINT ( 'NONE',  ( 3.999999999879999546, -3.000000000000000000, -135.0552959530000123 ) ) ;
#9828 = ORIENTED_EDGE ( 'NONE', *, *, #20561, .F. ) ;
#9829 = FACE_OUTER_BOUND ( 'NONE', #19239, .T. ) ;
#9830 = CARTESIAN_POINT ( 'NONE',  ( -12.50000000000000000, 45.50000000000000000, -136.0552959530000123 ) ) ;
#9831 = ORIENTED_EDGE ( 'NONE', *, *, #16241, .F. ) ;
#9832 = SURFACE_SIDE_STYLE ('',( #15561 ) ) ;
#9833 = DIRECTION ( 'NONE',  ( -2.509104035652851358E-12, 0.000000000000000000, 1.000000000000000000 ) ) ;
#9834 = VECTOR ( 'NONE', #6388, 1000.000000000000000 ) ;
#9835 = ORIENTED_EDGE ( 'NONE', *, *, #22549, .T. ) ;
#9836 = CARTESIAN_POINT ( 'NONE',  ( 15.50000000000000000, 36.50000000000000000, -137.0552959530000123 ) ) ;
#9837 = DIRECTION ( 'NONE',  ( 0.000000000000000000, 0.000000000000000000, -1.000000000000000000 ) ) ;
#9838 = ORIENTED_EDGE ( 'NONE', *, *, #3884, .T. ) ;
#9839 = VECTOR ( 'NONE', #8660, 1000.000000000000000 ) ;
#9840 = EDGE_CURVE ( 'NONE', #15915, #2624, #718, .T. ) ;
#9841 = CARTESIAN_POINT ( 'NONE',  ( -19.59255166827864159, 37.05126161859452338, -140.3061871182728169 ) ) ;
#9842 = ORIENTED_EDGE ( 'NONE', *, *, #633, .F. ) ;
#9843 = AXIS2_PLACEMENT_3D ( 'NONE', #2241, #18875, #18522 ) ;
#9844 = CARTESIAN_POINT ( 'NONE',  ( 1.133692148550000001, -51.00000000000000000, -137.0552959530000123 ) ) ;
#9845 = CIRCLE ( 'NONE', #11745, 2.000000000000000000 ) ;
#9846 = FACE_OUTER_BOUND ( 'NONE', #13128, .T. ) ;
#9847 = ORIENTED_EDGE ( 'NONE', *, *, #4591, .T. ) ;
#9848 = VECTOR ( 'NONE', #16237, 1000.000000000000000 ) ;
#9849 = DIRECTION ( 'NONE',  ( 0.9915498581664488054, 0.1297261684090585954, -4.315191440381949291E-12 ) ) ;
#9850 = CIRCLE ( 'NONE', #23170, 0.7500000000000006661 ) ;
#9851 = FACE_OUTER_BOUND ( 'NONE', #7677, .T. ) ;
#9852 = ORIENTED_EDGE ( 'NONE', *, *, #22160, .T. ) ;
#9853 = CARTESIAN_POINT ( 'NONE',  ( 25.94418247360000152, -46.04723021459999899, -149.5552959529999839 ) ) ;
#9854 = EDGE_LOOP ( 'NONE', ( #16381, #4291, #8165, #4117, #4573, #20559, #5422 ) ) ;
#9855 = CARTESIAN_POINT ( 'NONE',  ( 7.750000000000000000, -40.23606797749999942, -151.0552959529999839 ) ) ;
#9856 = DIRECTION ( 'NONE',  ( -1.734723475976805517E-14, -1.000000000000000000, 0.000000000000000000 ) ) ;
#9857 = ORIENTED_EDGE ( 'NONE', *, *, #5451, .F. ) ;
#9858 = ORIENTED_EDGE ( 'NONE', *, *, #21262, .T. ) ;
#9859 = VECTOR ( 'NONE', #14092, 1000.000000000000000 ) ;
#9860 = AXIS2_PLACEMENT_3D ( 'NONE', #1614, #21590, #8835 ) ;
#9861 = CARTESIAN_POINT ( 'NONE',  ( 1.500000000000000000, -3.500000000000000000, -150.0552959529999839 ) ) ;
#9862 = DIRECTION ( 'NONE',  ( 1.000000000000000000, 0.000000000000000000, -2.259303855112193560E-12 ) ) ;
#9863 = CIRCLE ( 'NONE', #3434, 6.000000000000001776 ) ;
#9864 = CIRCLE ( 'NONE', #7967, 1.499999999999999556 ) ;
#9865 = DIRECTION ( 'NONE',  ( -0.1107105301439589573, -0.9938526945756315234, 8.278459860356925655E-13 ) ) ;
#9866 = FACE_OUTER_BOUND ( 'NONE', #6060, .T. ) ;
#9867 = ORIENTED_EDGE ( 'NONE', *, *, #4844, .T. ) ;
#9868 = DIRECTION ( 'NONE',  ( 2.257749542879999954E-12, 0.000000000000000000, 1.000000000000000000 ) ) ;
#9869 = DIRECTION ( 'NONE',  ( 0.000000000000000000, 1.000000000000000000, 0.000000000000000000 ) ) ;
#9870 = CARTESIAN_POINT ( 'NONE',  ( 1.759100530420000030, -16.38142836440000139, -142.5552959529999839 ) ) ;
#9871 = CYLINDRICAL_SURFACE ( 'NONE', #3875, 2.000000000000003553 ) ;
#9872 = EDGE_CURVE ( 'NONE', #6188, #5644, #13251, .T. ) ;
#9873 = CARTESIAN_POINT ( 'NONE',  ( -23.24588518177116114, 41.24341284997103685, -143.7187626422519884 ) ) ;
#9874 = ADVANCED_FACE ( 'NONE', ( #2740 ), #12109, .T. ) ;
#9875 = CARTESIAN_POINT ( 'NONE',  ( -16.55827375301752014, 37.05535324331041380, -139.5705083843697594 ) ) ;
#9876 = DIRECTION ( 'NONE',  ( -5.094701932209999624E-24, -1.000000000000000000, 1.149947916579999802E-35 ) ) ;
#9877 = DIRECTION ( 'NONE',  ( 1.701177084980000217E-20, -2.602084704489999637E-17, 1.000000000000000000 ) ) ;
#9878 = DIRECTION ( 'NONE',  ( 1.000000000000000000, 0.000000000000000000, 0.000000000000000000 ) ) ;
#9879 = DIRECTION ( 'NONE',  ( 0.000000000000000000, 0.000000000000000000, 1.000000000000000000 ) ) ;
#9880 = CIRCLE ( 'NONE', #12555, 1.500000000000001332 ) ;
#9881 = ORIENTED_EDGE ( 'NONE', *, *, #7210, .F. ) ;
#9882 = CARTESIAN_POINT ( 'NONE',  ( -9.751275928061490461, 32.90710057661718935, -143.3218945113347615 ) ) ;
#9883 = CARTESIAN_POINT ( 'NONE',  ( -30.02199999990000023, 40.89711431700000333, -146.3052959529999839 ) ) ;
#9884 = DIRECTION ( 'NONE',  ( -1.000000000000000000, 0.000000000000000000, 0.000000000000000000 ) ) ;
#9885 = ORIENTED_EDGE ( 'NONE', *, *, #14437, .F. ) ;
#9886 = CARTESIAN_POINT ( 'NONE',  ( -22.00705883600000234, 37.05789963359999462, -148.1619053240000028 ) ) ;
#9887 = DIRECTION ( 'NONE',  ( 1.526468026909999897E-13, 8.159623473500000156E-13, 1.000000000000000000 ) ) ;
#9888 = ORIENTED_EDGE ( 'NONE', *, *, #6735, .T. ) ;
#9889 = CARTESIAN_POINT ( 'NONE',  ( -23.15277150037254827, 40.84402665608095617, -143.7661117063971972 ) ) ;
#9890 = DIRECTION ( 'NONE',  ( 2.507771768019999718E-12, 1.592654864069999939E-17, -1.000000000000000000 ) ) ;
#9891 = CARTESIAN_POINT ( 'NONE',  ( 1.924189958818393276, 14.53742485369798842, -150.0552959530000123 ) ) ;
#9892 = CARTESIAN_POINT ( 'NONE',  ( 5.792747474889999637, -16.92794981449999980, -144.5552959529999839 ) ) ;
#9893 = CARTESIAN_POINT ( 'NONE',  ( -27.11867290101618977, 36.95185637389148781, -147.5185143933870222 ) ) ;
#9894 = CIRCLE ( 'NONE', #3097, 8.176568160359998672 ) ;
#9895 = CARTESIAN_POINT ( 'NONE',  ( -9.562013113444269408, 37.00477621355919666, -148.7272342975821005 ) ) ;
#9896 = CARTESIAN_POINT ( 'NONE',  ( -9.005502668715839931, 40.51905748822048281, -141.9284054811836029 ) ) ;
#9897 = EDGE_CURVE ( 'NONE', #20935, #1717, #15452, .T. ) ;
#9898 = ORIENTED_EDGE ( 'NONE', *, *, #1065, .T. ) ;
#9899 = ADVANCED_FACE ( 'NONE', ( #4865 ), #19389, .F. ) ;
#9900 = DIRECTION ( 'NONE',  ( 1.000000000000000000, 0.000000000000000000, -2.257144641399999941E-12 ) ) ;
#9901 =( LENGTH_UNIT ( ) NAMED_UNIT ( * ) SI_UNIT ( .MILLI., .METRE. ) );
#9902 = ORIENTED_EDGE ( 'NONE', *, *, #15587, .T. ) ;
#9903 = PRODUCT_DEFINITION_SHAPE ( 'NONE', 'NONE',  #23554 ) ;
#9904 = PLANE ( 'NONE',  #15662 ) ;
#9905 = CARTESIAN_POINT ( 'NONE',  ( -27.16475626499999763, 37.90277890280000150, -148.4897851379999736 ) ) ;
#9906 = DIRECTION ( 'NONE',  ( 8.955190032050000935E-12, -9.104778821549999739E-13, 1.000000000000000000 ) ) ;
#9907 = ORIENTED_EDGE ( 'NONE', *, *, #10942, .F. ) ;
#9908 = LINE ( 'NONE', #15640, #18611 ) ;
#9909 = CARTESIAN_POINT ( 'NONE',  ( 0.000000000000000000, -40.23606797749999942, -150.0552959529999839 ) ) ;
#9910 = CIRCLE ( 'NONE', #13339, 3.499999999999999556 ) ;
#9911 = AXIS2_PLACEMENT_3D ( 'NONE', #20056, #12314, #10754 ) ;
#9912 = VERTEX_POINT ( 'NONE', #21060 ) ;
#9913 = CARTESIAN_POINT ( 'NONE',  ( -22.07763076357013077, 37.06632353693575510, -147.8362371614070696 ) ) ;
#9914 = CARTESIAN_POINT ( 'NONE',  ( -17.88596104465900183, 38.55815351507766309, -140.2676819153700762 ) ) ;
#9915 = CARTESIAN_POINT ( 'NONE',  ( 8.301573612353688958, 35.50007106174292915, -146.0553492493495753 ) ) ;
#9916 = ADVANCED_FACE ( 'NONE', ( #11876 ), #1529, .T. ) ;
#9917 = CARTESIAN_POINT ( 'NONE',  ( -13.86630785140000022, -50.50000000000000000, -137.0552959530000123 ) ) ;
#9918 = APPLICATION_CONTEXT ( 'automotive_design' ) ;
#9919 = CARTESIAN_POINT ( 'NONE',  ( -25.11008055915115378, 33.57149262957015878, -144.4317693003656586 ) ) ;
#9920 = CARTESIAN_POINT ( 'NONE',  ( 18.95053822279999878, -50.50000000000000000, -143.0552959529999839 ) ) ;
#9921 = ORIENTED_EDGE ( 'NONE', *, *, #19681, .T. ) ;
#9922 = CARTESIAN_POINT ( 'NONE',  ( -33.36626399469999882, 47.50000000000000000, -138.5552959529999839 ) ) ;
#9923 = AXIS2_PLACEMENT_3D ( 'NONE', #17022, #11303, #18579 ) ;
#9924 = EDGE_CURVE ( 'NONE', #13504, #4170, #19508, .T. ) ;
#9925 = VECTOR ( 'NONE', #1102, 1000.000000000000000 ) ;
#9926 = AXIS2_PLACEMENT_3D ( 'NONE', #395, #9877, #13458 ) ;
#9927 = ORIENTED_EDGE ( 'NONE', *, *, #3251, .F. ) ;
#9928 = SURFACE_STYLE_USAGE ( .BOTH. , #916 ) ;
#9929 = ORIENTED_EDGE ( 'NONE', *, *, #11917, .T. ) ;
#9930 = CARTESIAN_POINT ( 'NONE',  ( 32.50000000000000000, 26.96379895119999759, -137.0552959530000123 ) ) ;
#9931 = VERTEX_POINT ( 'NONE', #8536 ) ;
#9932 = LINE ( 'NONE', #12075, #2675 ) ;
#9933 = EDGE_LOOP ( 'NONE', ( #18784, #20954, #17941, #21567 ) ) ;
#9934 = ORIENTED_EDGE ( 'NONE', *, *, #19440, .T. ) ;
#9935 = LINE ( 'NONE', #15672, #17853 ) ;
#9936 = EDGE_CURVE ( 'NONE', #19743, #10194, #19762, .T. ) ;
#9937 = DIRECTION ( 'NONE',  ( 2.842170943040000002E-14, 3.552713678800000097E-13, 1.000000000000000000 ) ) ;
#9938 = FACE_OUTER_BOUND ( 'NONE', #419, .T. ) ;
#9939 = LINE ( 'NONE', #4839, #21234 ) ;
#9940 = ADVANCED_FACE ( 'NONE', ( #23190 ), #11750, .F. ) ;
#9941 = CARTESIAN_POINT ( 'NONE',  ( -7.529689113779999943, 37.05876528330000497, -139.9906690790000141 ) ) ;
#9942 = CARTESIAN_POINT ( 'NONE',  ( -9.747014461865537882, 38.96264327593980425, -148.3170967394802631 ) ) ;
#9943 = ORIENTED_EDGE ( 'NONE', *, *, #21704, .F. ) ;
#9944 = CARTESIAN_POINT ( 'NONE',  ( -27.58110728279999790, 34.24318910290000417, -147.7245096240000066 ) ) ;
#9945 = AXIS2_PLACEMENT_3D ( 'NONE', #16512, #2367, #15076 ) ;
#9946 = EDGE_CURVE ( 'NONE', #5050, #14322, #2658, .T. ) ;
#9947 = CARTESIAN_POINT ( 'NONE',  ( 9.105676901957313163, 38.37253232039734741, -146.1448649138488634 ) ) ;
#9948 = EDGE_CURVE ( 'NONE', #18719, #22568, #8179, .T. ) ;
#9949 = CARTESIAN_POINT ( 'NONE',  ( 25.11896946143725984, 38.01480899505094868, -150.0552959529999839 ) ) ;
#9950 = ORIENTED_EDGE ( 'NONE', *, *, #17963, .T. ) ;
#9951 = EDGE_CURVE ( 'NONE', #20880, #634, #1070, .T. ) ;
#9952 = EDGE_CURVE ( 'NONE', #22607, #760, #22840, .T. ) ;
#9953 = FACE_OUTER_BOUND ( 'NONE', #21098, .T. ) ;
#9954 = PLANE ( 'NONE',  #1583 ) ;
#9955 = EDGE_LOOP ( 'NONE', ( #21407, #9963, #14385, #18825 ) ) ;
#9956 = CARTESIAN_POINT ( 'NONE',  ( 31.50000000000000000, 0.000000000000000000, -137.0552959530000123 ) ) ;
#9957 = ORIENTED_EDGE ( 'NONE', *, *, #17641, .T. ) ;
#9958 = DIRECTION ( 'NONE',  ( 1.000000000000000000, 0.000000000000000000, -2.257453483404485639E-12 ) ) ;
#9959 = DIRECTION ( 'NONE',  ( 0.9896415801065049367, -0.1435602414469282218, -8.993136838065500309E-12 ) ) ;
#9960 = ORIENTED_EDGE ( 'NONE', *, *, #17254, .F. ) ;
#9961 = CARTESIAN_POINT ( 'NONE',  ( -15.32446908972706190, 41.39793051967586734, -143.4941841294994447 ) ) ;
#9962 = CARTESIAN_POINT ( 'NONE',  ( -25.17849978636914443, 32.75955230985957201, -146.5550213843877998 ) ) ;
#9963 = ORIENTED_EDGE ( 'NONE', *, *, #14649, .F. ) ;
#9964 = SHAPE_DEFINITION_REPRESENTATION ( #8269, #7672 ) ;
#9965 = VECTOR ( 'NONE', #10520, 1000.000000000000000 ) ;
#9966 = DIRECTION ( 'NONE',  ( 0.000000000000000000, 0.000000000000000000, 1.000000000000000000 ) ) ;
#9967 = ORIENTED_EDGE ( 'NONE', *, *, #10137, .F. ) ;
#9968 = DIRECTION ( 'NONE',  ( 2.507771768019999718E-12, 1.592654864209999947E-17, -1.000000000000000000 ) ) ;
#9969 = DIRECTION ( 'NONE',  ( -0.06206811009758109871, 0.9980719161006958995, -8.049146049297549005E-13 ) ) ;
#9970 = ORIENTED_EDGE ( 'NONE', *, *, #2853, .T. ) ;
#9971 = CARTESIAN_POINT ( 'NONE',  ( -6.547730170579999509, -18.66441632429999942, -147.5552959529999839 ) ) ;
#9972 = ORIENTED_EDGE ( 'NONE', *, *, #13240, .F. ) ;
#9973 = FACE_BOUND ( 'NONE', #14182, .T. ) ;
#9974 = DIRECTION ( 'NONE',  ( -0.7633862853691523176, 0.6459422414661291079, 0.000000000000000000 ) ) ;
#9975 = ORIENTED_EDGE ( 'NONE', *, *, #18080, .F. ) ;
#9976 = PRODUCT_DEFINITION_SHAPE ( 'NONE', 'NONE',  #781 ) ;
#9977 = EDGE_CURVE ( 'NONE', #2118, #20985, #11279, .T. ) ;
#9978 = VERTEX_POINT ( 'NONE', #1315 ) ;
#9979 = CARTESIAN_POINT ( 'NONE',  ( 5.285243653077836612, -0.5780819699950525692, -150.0552959529999839 ) ) ;
#9980 = CARTESIAN_POINT ( 'NONE',  ( 0.1832000607640000001, 0.4999999999990000776, -150.0552959529999839 ) ) ;
#9981 = CARTESIAN_POINT ( 'NONE',  ( -8.916553640509999212, -11.88594259849999979, -143.5552959529999839 ) ) ;
#9982 = LINE ( 'NONE', #10095, #8702 ) ;
#9983 = ORIENTED_EDGE ( 'NONE', *, *, #5728, .F. ) ;
#9984 = CARTESIAN_POINT ( 'NONE',  ( 32.00000000000000000, 39.80430157320000006, -150.0552959529999839 ) ) ;
#9985 = CARTESIAN_POINT ( 'NONE',  ( 7.228490359739999427, -13.33508289800000135, -145.5552959529999839 ) ) ;
#9986 = FACE_OUTER_BOUND ( 'NONE', #6959, .T. ) ;
#9987 = FACE_OUTER_BOUND ( 'NONE', #15596, .T. ) ;
#9988 = LINE ( 'NONE', #19410, #7643 ) ;
#9989 = CARTESIAN_POINT ( 'NONE',  ( -7.826190453620396781, -26.58762194555488989, -147.5552959530076009 ) ) ;
#9990 = ORIENTED_EDGE ( 'NONE', *, *, #254, .F. ) ;
#9991 = FACE_OUTER_BOUND ( 'NONE', #15571, .T. ) ;
#9992 = CARTESIAN_POINT ( 'NONE',  ( -16.50205712333324826, 33.47704857309710036, -144.2911601313269898 ) ) ;
#9993 = CARTESIAN_POINT ( 'NONE',  ( -4.609334941132099850, 37.98062953722018875, -139.6349070798746936 ) ) ;
#9994 = CARTESIAN_POINT ( 'NONE',  ( -21.35824191589999899, -4.000000000000000000, -144.8157682190000060 ) ) ;
#9995 = PRODUCT_DEFINITION_FORMATION_WITH_SPECIFIED_SOURCE ( 'ANY', '', #4785, .NOT_KNOWN. ) ;
#9996 = CARTESIAN_POINT ( 'NONE',  ( -15.00000000000000000, -43.00000000000000000, -140.0552959529999839 ) ) ;
#9997 = EDGE_LOOP ( 'NONE', ( #8521, #5939, #18034, #19896 ) ) ;
#9998 = CARTESIAN_POINT ( 'NONE',  ( -9.394775000179999225, 34.25903911019999981, -147.4808749560000081 ) ) ;
#9999 = VECTOR ( 'NONE', #22079, 1000.000000000000000 ) ;
#10000 = CARTESIAN_POINT ( 'NONE',  ( -21.35824191589999899, -32.75000000000000000, -146.3157682190075093 ) ) ;
#10001 = DIRECTION ( 'NONE',  ( 2.602084747549999882E-17, -1.000000000000000000, -5.873289694040000105E-29 ) ) ;
#10002 = EDGE_LOOP ( 'NONE', ( #22288, #12519, #2858, #22933 ) ) ;
#10003 = FACE_OUTER_BOUND ( 'NONE', #10530, .T. ) ;
#10004 = EDGE_CURVE ( 'NONE', #15489, #17671, #6757, .T. ) ;
#10005 = CARTESIAN_POINT ( 'NONE',  ( -4.499999999929999994, 31.50000000000000000, -138.0552959530000123 ) ) ;
#10006 = CARTESIAN_POINT ( 'NONE',  ( 8.100000000049998761, 39.46779253580000102, -148.0552959529999839 ) ) ;
#10007 = ORIENTED_EDGE ( 'NONE', *, *, #3769, .F. ) ;
#10008 = CARTESIAN_POINT ( 'NONE',  ( -23.68366236538869174, 38.48614108665564970, -140.6202320859351573 ) ) ;
#10009 = DIRECTION ( 'NONE',  ( 1.000000000000000000, 0.000000000000000000, -2.262368070660000099E-12 ) ) ;
#10010 = FACE_OUTER_BOUND ( 'NONE', #21382, .T. ) ;
#10011 = CARTESIAN_POINT ( 'NONE',  ( 6.500000000149999124, 28.50000000000000000, -143.5552959529999839 ) ) ;
#10012 = CARTESIAN_POINT ( 'NONE',  ( -10.07619956174958098, 36.21908991358723995, -147.8536995440399835 ) ) ;
#10013 = CARTESIAN_POINT ( 'NONE',  ( 5.792747474879999636, -16.92794981449999980, -145.5552959529999839 ) ) ;
#10014 = CARTESIAN_POINT ( 'NONE',  ( -8.712023184228140593, 38.57885015678616014, -140.3122811006342090 ) ) ;
#10015 = AXIS2_PLACEMENT_3D ( 'NONE', #12874, #18127, #1611 ) ;
#10016 = ORIENTED_EDGE ( 'NONE', *, *, #14598, .T. ) ;
#10017 = CARTESIAN_POINT ( 'NONE',  ( -21.93648690847360072, 37.04947573026750973, -148.4875734863011303 ) ) ;
#10018 =( LENGTH_UNIT ( ) NAMED_UNIT ( * ) SI_UNIT ( .MILLI., .METRE. ) );
#10019 = EDGE_LOOP ( 'NONE', ( #6418, #9975 ) ) ;
#10020 = CARTESIAN_POINT ( 'NONE',  ( -7.080966237668673280, 35.02109009467289980, -146.9136362634284012 ) ) ;
#10021 = DIRECTION ( 'NONE',  ( -1.000000000000000000, 0.000000000000000000, -2.516505522483685870E-12 ) ) ;
#10022 = CARTESIAN_POINT ( 'NONE',  ( 10.68320006080000084, -21.50000000000000000, -148.5552959529999839 ) ) ;
#10023 = EDGE_LOOP ( 'NONE', ( #15549, #6024, #8591, #22429, #10260 ) ) ;
#10024 = CYLINDRICAL_SURFACE ( 'NONE', #6838, 7.500000000000005329 ) ;
#10025 = CARTESIAN_POINT ( 'NONE',  ( -15.26331651089999930, 39.75437292659999855, -147.8043400740000095 ) ) ;
#10026 = ORIENTED_EDGE ( 'NONE', *, *, #20248, .T. ) ;
#10027 = CARTESIAN_POINT ( 'NONE',  ( -34.50000000000000000, 27.00000000000000000, -141.5552959529999839 ) ) ;
#10028 = EDGE_CURVE ( 'NONE', #10724, #9007, #20087, .T. ) ;
#10029 = VECTOR ( 'NONE', #2881, 1000.000000000000000 ) ;
#10030 = CARTESIAN_POINT ( 'NONE',  ( -17.84118295813777522, 39.08206477522340805, -141.0250297803352453 ) ) ;
#10031 = ADVANCED_FACE ( 'NONE', ( #2021 ), #9243, .F. ) ;
#10032 = CARTESIAN_POINT ( 'NONE',  ( 8.108968687586248336, 38.44920563369909416, -146.0924816361253704 ) ) ;
#10033 = PLANE ( 'NONE',  #1749 ) ;
#10034 = CARTESIAN_POINT ( 'NONE',  ( -25.91744746520000220, 33.58572460659999592, -142.1592104600000255 ) ) ;
#10035 = CARTESIAN_POINT ( 'NONE',  ( -34.50000000000000000, 26.00000000000000000, -146.5552959529999839 ) ) ;
#10036 = ORIENTED_EDGE ( 'NONE', *, *, #4924, .T. ) ;
#10037 = DIRECTION ( 'NONE',  ( -2.507771768023035002E-12, -1.592654560756634986E-17, 1.000000000000000000 ) ) ;
#10038 = EDGE_LOOP ( 'NONE', ( #18067, #20928, #19361, #11129, #12909, #17676, #7557 ) ) ;
#10039 = CARTESIAN_POINT ( 'NONE',  ( -27.11867290101617556, 36.95185637389150912, -147.5185143933871075 ) ) ;
#10040 = ORIENTED_EDGE ( 'NONE', *, *, #4708, .F. ) ;
#10041 = LINE ( 'NONE', #9930, #12499 ) ;
#10042 = ORIENTED_EDGE ( 'NONE', *, *, #17578, .T. ) ;
#10043 = VECTOR ( 'NONE', #9739, 1000.000000000000000 ) ;
#10044 = CARTESIAN_POINT ( 'NONE',  ( -0.6175362654355562864, 22.91577772018733583, -136.0552959529986197 ) ) ;
#10045 = ORIENTED_EDGE ( 'NONE', *, *, #4032, .T. ) ;
#10046 = ADVANCED_BREP_SHAPE_REPRESENTATION ( '', ( #4113, #5025 ), #5047 ) ;
#10047 = VERTEX_POINT ( 'NONE', #18068 ) ;
#10048 = LINE ( 'NONE', #3065, #17074 ) ;
#10049 = CARTESIAN_POINT ( 'NONE',  ( -18.95027878879999861, 36.16636532760000478, -148.4341920939999966 ) ) ;
#10050 = CYLINDRICAL_SURFACE ( 'NONE', #22525, 2.500000000000000000 ) ;
#10051 = CARTESIAN_POINT ( 'NONE',  ( 8.500000000060001781, 37.00000000000000000, -142.5552959529999839 ) ) ;
#10052 = CARTESIAN_POINT ( 'NONE',  ( -8.208807763331680718, 34.49436158495667826, -140.8229124834255970 ) ) ;
#10053 = CARTESIAN_POINT ( 'NONE',  ( -8.869124888310000898, 38.72872035620000020, -148.0517159070000162 ) ) ;
#10054 = ORIENTED_EDGE ( 'NONE', *, *, #11164, .F. ) ;
#10055 = PLANE ( 'NONE',  #15528 ) ;
#10056 = EDGE_CURVE ( 'NONE', #14263, #7697, #21805, .T. ) ;
#10057 = CYLINDRICAL_SURFACE ( 'NONE', #3019, 2.499999999999998668 ) ;
#10058 = AXIS2_PLACEMENT_3D ( 'NONE', #1443, #8445, #11894 ) ;
#10059 = DIRECTION ( 'NONE',  ( -1.000000000000000000, 0.000000000000000000, 2.273736754430000208E-12 ) ) ;
#10060 = VERTEX_POINT ( 'NONE', #14721 ) ;
#10061 = EDGE_CURVE ( 'NONE', #6635, #22142, #5097, .T. ) ;
#10062 = DIRECTION ( 'NONE',  ( -0.1000233216789610108, -0.9949850929136109245, 3.559993607998610461E-13 ) ) ;
#10063 = CARTESIAN_POINT ( 'NONE',  ( -31.00000000000000000, 37.00000000000000000, -149.0552959529999839 ) ) ;
#10064 = ORIENTED_EDGE ( 'NONE', *, *, #3720, .F. ) ;
#10065 = FILL_AREA_STYLE_COLOUR ( '', #21205 ) ;
#10066 = DIRECTION ( 'NONE',  ( 2.257171095940000041E-12, -7.494005416210000121E-16, 1.000000000000000000 ) ) ;
#10067 = ORIENTED_EDGE ( 'NONE', *, *, #3001, .F. ) ;
#10068 = DIRECTION ( 'NONE',  ( -0.7633862853691523176, 0.6459422414661291079, 0.000000000000000000 ) ) ;
#10069 = CARTESIAN_POINT ( 'NONE',  ( 21.65635984007526105, -22.89900052719454493, -150.0552959529999839 ) ) ;
#10070 = ORIENTED_EDGE ( 'NONE', *, *, #20012, .T. ) ;
#10071 = CARTESIAN_POINT ( 'NONE',  ( -15.23014954472039939, 40.61563974024299029, -144.3756286147995809 ) ) ;
#10072 = CARTESIAN_POINT ( 'NONE',  ( -24.16551117127903936, 36.07182940195683329, -148.2420083170896135 ) ) ;
#10073 = VERTEX_POINT ( 'NONE', #16284 ) ;
#10074 = EDGE_CURVE ( 'NONE', #10304, #12120, #21158, .T. ) ;
#10075 = CARTESIAN_POINT ( 'NONE',  ( 8.750000000030000891, -37.98606797749999942, -136.5552959530000123 ) ) ;
#10076 = ORIENTED_EDGE ( 'NONE', *, *, #8408, .F. ) ;
#10077 = CARTESIAN_POINT ( 'NONE',  ( 19.59648046430000079, 50.76338628540000286, -150.0552959529999839 ) ) ;
#10078 = EDGE_CURVE ( 'NONE', #6969, #2758, #23420, .T. ) ;
#10079 = VECTOR ( 'NONE', #19015, 1000.000000000000000 ) ;
#10080 = PLANE ( 'NONE',  #1258 ) ;
#10081 = ORIENTED_EDGE ( 'NONE', *, *, #21477, .F. ) ;
#10082 = AXIS2_PLACEMENT_3D ( 'NONE', #22555, #17309, #22789 ) ;
#10083 = CARTESIAN_POINT ( 'NONE',  ( -6.165211177139999776, -15.11551140080000089, -143.0552959529999839 ) ) ;
#10084 = EDGE_CURVE ( 'NONE', #2213, #6279, #3314, .T. ) ;
#10085 = ORIENTED_EDGE ( 'NONE', *, *, #22460, .F. ) ;
#10086 = LINE ( 'NONE', #12238, #22372 ) ;
#10087 = ADVANCED_FACE ( 'NONE', ( #19740 ), #12194, .F. ) ;
#10088 = CARTESIAN_POINT ( 'NONE',  ( -25.12153080219999879, 33.08100675569999538, -141.7696838820000096 ) ) ;
#10089 = ORIENTED_EDGE ( 'NONE', *, *, #3052, .F. ) ;
#10090 = EDGE_LOOP ( 'NONE', ( #7731, #7330 ) ) ;
#10091 = DIRECTION ( 'NONE',  ( 1.000000000000000000, 0.000000000000000000, -2.256131789327549967E-12 ) ) ;
#10092 = DIRECTION ( 'NONE',  ( 0.000000000000000000, 0.000000000000000000, 1.000000000000000000 ) ) ;
#10093 = EDGE_CURVE ( 'NONE', #12394, #2513, #17092, .T. ) ;
#10094 = CARTESIAN_POINT ( 'NONE',  ( -46.49999999989999822, 37.00000000000000000, -144.0552959529999839 ) ) ;
#10095 = CARTESIAN_POINT ( 'NONE',  ( 31.50000000000000000, -40.03620104880000241, -143.0552959529999839 ) ) ;
#10096 = PRODUCT_DEFINITION_SHAPE ( 'NONE', 'NONE',  #23549 ) ;
#10097 = AXIS2_PLACEMENT_3D ( 'NONE', #10538, #23531, #10894 ) ;
#10098 = ORIENTED_EDGE ( 'NONE', *, *, #17787, .F. ) ;
#10099 = CARTESIAN_POINT ( 'NONE',  ( -34.50000000000000000, -64.50000000000000000, -144.0552959529999839 ) ) ;
#10100 = CIRCLE ( 'NONE', #11608, 14.99999999999999822 ) ;
#10101 = CARTESIAN_POINT ( 'NONE',  ( -22.10824191589999899, -34.50000000000000000, -144.8157682190000060 ) ) ;
#10102 = EDGE_CURVE ( 'NONE', #7870, #3729, #12935, .T. ) ;
#10103 = DIRECTION ( 'NONE',  ( 0.000000000000000000, 4.009147065150000317E-51, -1.000000000000000000 ) ) ;
#10104 = LINE ( 'NONE', #19164, #14731 ) ;
#10105 = CARTESIAN_POINT ( 'NONE',  ( 14.71940181160194427, 39.42378041200770156, -136.0552959530332373 ) ) ;
#10106 = LINE ( 'NONE', #8327, #23503 ) ;
#10107 = ORIENTED_EDGE ( 'NONE', *, *, #6259, .T. ) ;
#10108 = CARTESIAN_POINT ( 'NONE',  ( 0.1832000607640000001, 0.4999999999990000776, -148.5552959529999839 ) ) ;
#10109 = EDGE_CURVE ( 'NONE', #18841, #4401, #20213, .T. ) ;
#10110 = DIRECTION ( 'NONE',  ( 1.526468026909999897E-13, 8.159623473500000156E-13, 1.000000000000000000 ) ) ;
#10111 = EDGE_CURVE ( 'NONE', #7689, #16462, #18416, .T. ) ;
#10112 = LINE ( 'NONE', #15722, #12988 ) ;
#10113 = CARTESIAN_POINT ( 'NONE',  ( -4.510059210066960311, 37.06110843049349768, -139.6225057176258133 ) ) ;
#10114 = DIRECTION ( 'NONE',  ( 1.000000000000000000, 0.000000000000000000, -2.257453483404485639E-12 ) ) ;
#10115 = EDGE_CURVE ( 'NONE', #20464, #6561, #19512, .T. ) ;
#10116 = ORIENTED_EDGE ( 'NONE', *, *, #12838, .T. ) ;
#10117 = CARTESIAN_POINT ( 'NONE',  ( -8.931798216468004981, 36.92954985151560265, -147.9669232058148793 ) ) ;
#10118 = CARTESIAN_POINT ( 'NONE',  ( 19.86977406280000125, -31.59375768830000197, -147.5552959529999839 ) ) ;
#10119 = CARTESIAN_POINT ( 'NONE',  ( 4.109383212426824805, -2.038350857853872711, -150.0552959529999839 ) ) ;
#10120 = ORIENTED_EDGE ( 'NONE', *, *, #1643, .F. ) ;
#10121 = DIRECTION ( 'NONE',  ( 1.000000000000000000, 0.000000000000000000, -2.257453483404484831E-12 ) ) ;
#10122 = PLANE ( 'NONE',  #18216 ) ;
#10123 = PLANE ( 'NONE',  #7192 ) ;
#10124 = ORIENTED_EDGE ( 'NONE', *, *, #19412, .T. ) ;
#10125 = CARTESIAN_POINT ( 'NONE',  ( -13.91784526144543932, 35.46792342014339994, -140.7554205113700050 ) ) ;
#10126 = LINE ( 'NONE', #8352, #1763 ) ;
#10127 = CARTESIAN_POINT ( 'NONE',  ( -0.7600837004312114287, 18.55411937531333777, -150.0552959529999839 ) ) ;
#10128 = LINE ( 'NONE', #19187, #20873 ) ;
#10129 = CARTESIAN_POINT ( 'NONE',  ( -10.98352009339088653, 32.87162191921307652, -143.4565451244976657 ) ) ;
#10130 = CARTESIAN_POINT ( 'NONE',  ( -25.35824191590000254, -34.50000000000000000, -144.8157682190000060 ) ) ;
#10131 = AXIS2_PLACEMENT_3D ( 'NONE', #198, #16603, #7443 ) ;
#10132 = CARTESIAN_POINT ( 'NONE',  ( 9.593637377583139170, -37.00248504027853613, -150.0552959529999839 ) ) ;
#10133 = ORIENTED_EDGE ( 'NONE', *, *, #2829, .T. ) ;
#10134 = VECTOR ( 'NONE', #5727, 1000.000000000000000 ) ;
#10135 =( NAMED_UNIT ( * ) SI_UNIT ( $, .STERADIAN. ) SOLID_ANGLE_UNIT ( ) );
#10136 = EDGE_CURVE ( 'NONE', #13352, #13163, #22794, .T. ) ;
#10137 = EDGE_CURVE ( 'NONE', #2396, #17085, #16971, .T. ) ;
#10138 = ORIENTED_EDGE ( 'NONE', *, *, #20730, .T. ) ;
#10139 = CARTESIAN_POINT ( 'NONE',  ( -7.404748324622609346, 34.90846072521996746, -141.2185729789256357 ) ) ;
#10140 = DIRECTION ( 'NONE',  ( 1.526468026909999897E-13, 8.159623473500000156E-13, 1.000000000000000000 ) ) ;
#10141 = CARTESIAN_POINT ( 'NONE',  ( -20.55310894649999653, 37.85259822169999921, -139.7937414779999870 ) ) ;
#10142 = B_SPLINE_CURVE_WITH_KNOTS ( 'NONE', 3,
 ( #18378, #11452, #18733, #13242, #13014, #2089, #15152, #20516, #11210, #9308 ),
 .UNSPECIFIED., .F., .F.,
 ( 4, 2, 2, 2, 4 ),
 ( 0.000000000000000000, 0.2499999999999997224, 0.5000000000000000000, 0.7500000000000002220, 1.000000000000000000 ),
 .UNSPECIFIED. ) ;
#10143 = VERTEX_POINT ( 'NONE', #2366 ) ;
#10144 = DIRECTION ( 'NONE',  ( 1.000000000000000000, 0.000000000000000000, -2.253752739989067373E-12 ) ) ;
#10145 = LINE ( 'NONE', #6477, #17095 ) ;
#10146 = ORIENTED_EDGE ( 'NONE', *, *, #4143, .T. ) ;
#10147 = DIRECTION ( 'NONE',  ( -2.257171095940000041E-12, 0.000000000000000000, -1.000000000000000000 ) ) ;
#10148 = VECTOR ( 'NONE', #19012, 1000.000000000000000 ) ;
#10149 = CARTESIAN_POINT ( 'NONE',  ( -17.53224077489999999, 39.64394931100000008, -140.2973660050000149 ) ) ;
#10150 = MECHANICAL_DESIGN_GEOMETRIC_PRESENTATION_REPRESENTATION (  '', ( #306 ), #16631 ) ;
#10151 = DIRECTION ( 'NONE',  ( 0.000000000000000000, 1.000000000000000000, 0.000000000000000000 ) ) ;
#10152 = CARTESIAN_POINT ( 'NONE',  ( 7.009850708823739396, 36.80024279011028199, -146.5492378968398555 ) ) ;
#10153 = CARTESIAN_POINT ( 'NONE',  ( 12.68320006090000085, -24.50000000000000000, -150.0552959529999839 ) ) ;
#10154 = CARTESIAN_POINT ( 'NONE',  ( -25.98284937189643529, 35.54018228806221913, -140.8314003423548968 ) ) ;
#10155 = DIRECTION ( 'NONE',  ( 1.000000000000000000, 0.000000000000000000, -4.510774274160000731E-12 ) ) ;
#10156 = CARTESIAN_POINT ( 'NONE',  ( -11.59046614940708153, 39.86879823875771933, -140.2222977132334165 ) ) ;
#10157 = ORIENTED_EDGE ( 'NONE', *, *, #21023, .T. ) ;
#10158 = DIRECTION ( 'NONE',  ( -1.000000000000000000, 0.000000000000000000, 0.000000000000000000 ) ) ;
#10159 = PRODUCT_DEFINITION_CONTEXT ( 'detailed design', #14809, 'design' ) ;
#10160 = ADVANCED_FACE ( 'NONE', ( #9586 ), #7802, .F. ) ;
#10162 = VERTEX_POINT ( 'NONE', #20785 ) ;
#10161 = VECTOR ( 'NONE', #22295, 1000.000000000000114 ) ;
#10163 = CARTESIAN_POINT ( 'NONE',  ( -27.49486172903679204, 36.99676060752978657, -147.4549925864818931 ) ) ;
#10164 = ORIENTED_EDGE ( 'NONE', *, *, #5038, .F. ) ;
#10165 = EDGE_CURVE ( 'NONE', #18702, #1936, #17574, .T. ) ;
#10166 = LINE ( 'NONE', #13761, #10969 ) ;
#10167 = VECTOR ( 'NONE', #560, 1000.000000000000000 ) ;
#10168 = VERTEX_POINT ( 'NONE', #8512 ) ;
#10169 = PLANE ( 'NONE',  #17098 ) ;
#10170 = EDGE_CURVE ( 'NONE', #16332, #2684, #6730, .T. ) ;
#10171 = ORIENTED_EDGE ( 'NONE', *, *, #15122, .F. ) ;
#10172 = VERTEX_POINT ( 'NONE', #4717 ) ;
#10173 = FACE_OUTER_BOUND ( 'NONE', #2264, .T. ) ;
#10174 = CARTESIAN_POINT ( 'NONE',  ( -19.29243665411954822, 35.40841497951669936, -148.0186320824420818 ) ) ;
#10175 = CARTESIAN_POINT ( 'NONE',  ( -11.31333818511670408, 38.44169350299409160, -140.8806452754523093 ) ) ;
#10176 = CARTESIAN_POINT ( 'NONE',  ( -12.41698512465752380, 36.98746477262142918, -147.4237781435811030 ) ) ;
#10177 = LINE ( 'NONE', #19358, #17114 ) ;
#10178 = CARTESIAN_POINT ( 'NONE',  ( -9.674592407111139991, 39.37273218265404040, -147.1879168908690190 ) ) ;
#10179 = ORIENTED_EDGE ( 'NONE', *, *, #18826, .T. ) ;
#10180 = PLANE ( 'NONE',  #13620 ) ;
#10181 = VECTOR ( 'NONE', #3126, 1000.000000000000000 ) ;
#10182 = CARTESIAN_POINT ( 'NONE',  ( 9.189953965651115553, 38.33228193160125130, -146.1707627155817590 ) ) ;
#10183 = VECTOR ( 'NONE', #21083, 1000.000000000000000 ) ;
#10184 = CARTESIAN_POINT ( 'NONE',  ( 24.33948587669790342, 34.09808825513669461, -150.0552959529999839 ) ) ;
#10185 = EDGE_LOOP ( 'NONE', ( #9460, #4095, #9168, #16218 ) ) ;
#10186 = DIRECTION ( 'NONE',  ( 0.9991304227374304681, 0.04169410462551791791, -4.421380363651902035E-14 ) ) ;
#10187 = DIRECTION ( 'NONE',  ( -2.602084747549999882E-17, 1.000000000000000000, 5.873289694040000105E-29 ) ) ;
#10188 = VERTEX_POINT ( 'NONE', #21029 ) ;
#10189 = DIRECTION ( 'NONE',  ( 2.257083409060000051E-12, 0.000000000000000000, 1.000000000000000000 ) ) ;
#10190 = DIRECTION ( 'NONE',  ( 2.257144641399999941E-12, -4.009147065140000298E-51, 1.000000000000000000 ) ) ;
#10191 = VERTEX_POINT ( 'NONE', #15780 ) ;
#10192 = CARTESIAN_POINT ( 'NONE',  ( -22.92066848221891107, 37.01209555893892400, -139.3757315020603187 ) ) ;
#10193 = CARTESIAN_POINT ( 'NONE',  ( -33.50000000000000000, 48.00000000000000000, -150.5552959529999839 ) ) ;
#10194 = VERTEX_POINT ( 'NONE', #21263 ) ;
#10195 = CARTESIAN_POINT ( 'NONE',  ( -14.50908993386010870, 36.94185792196182661, -140.4668331870292377 ) ) ;
#10196 = CARTESIAN_POINT ( 'NONE',  ( -25.42000568121191151, 32.21859392833894731, -144.6204194868284958 ) ) ;
#10197 = ADVANCED_FACE ( 'NONE', ( #13990 ), #18999, .T. ) ;
#10198 = VERTEX_POINT ( 'NONE', #19354 ) ;
#10199 = SHAPE_REPRESENTATION_RELATIONSHIP ( 'NONE' , 'NONE' ,  #14082, #23143 ) ;
#10200 = VECTOR ( 'NONE', #9974, 1000.000000000000227 ) ;
#10201 = LINE ( 'NONE', #17921, #15728 ) ;
#10202 = EDGE_LOOP ( 'NONE', ( #11869, #12356, #5027 ) ) ;
#10203 = DIRECTION ( 'NONE',  ( 1.000000000000000000, 0.000000000000000000, 2.516505522483685870E-12 ) ) ;
#10204 = AXIS2_PLACEMENT_3D ( 'NONE', #15417, #1163, #18992 ) ;
#10205 = CARTESIAN_POINT ( 'NONE',  ( -8.594304764349999459, -10.75357442870000035, -145.0552959529999839 ) ) ;
#10206 = ORIENTED_EDGE ( 'NONE', *, *, #15367, .T. ) ;
#10207 = CARTESIAN_POINT ( 'NONE',  ( 8.500000000060001781, 37.00000000000000000, -142.5552959529999839 ) ) ;
#10208 = CIRCLE ( 'NONE', #11336, 2.499999999999998668 ) ;
#10209 = PRODUCT_DEFINITION ( 'UNKNOWN', '', #6211, #17316 ) ;
#10210 = VECTOR ( 'NONE', #13550, 1000.000000000000000 ) ;
#10211 = CARTESIAN_POINT ( 'NONE',  ( -35.20609992760000040, 11.31289830180000067, -143.5552959529999839 ) ) ;
#10212 = EDGE_CURVE ( 'NONE', #10651, #12978, #756, .T. ) ;
#10213 = CARTESIAN_POINT ( 'NONE',  ( 8.645354125658261779, -29.00058528980708417, -146.5552959529681232 ) ) ;
#10214 = ORIENTED_EDGE ( 'NONE', *, *, #2989, .T. ) ;
#10215 = CARTESIAN_POINT ( 'NONE',  ( 0.5000000001500000124, 16.89444872450000190, -143.5552959529999839 ) ) ;
#10216 = AXIS2_PLACEMENT_3D ( 'NONE', #22345, #3706, #1944 ) ;
#10217 = ADVANCED_FACE ( 'NONE', ( #10173 ), #17444, .T. ) ;
#10218 = CARTESIAN_POINT ( 'NONE',  ( 19.13369214879999802, 50.49999999980000354, -150.0552959529999839 ) ) ;
#10219 = AXIS2_PLACEMENT_3D ( 'NONE', #17524, #11676, #22762 ) ;
#10220 = CARTESIAN_POINT ( 'NONE',  ( -14.78241661194416068, 39.12140059992913166, -147.0349140006744904 ) ) ;
#10221 = CARTESIAN_POINT ( 'NONE',  ( 19.45666326950000169, -50.88169314249999786, -136.0552959530000123 ) ) ;
#10222 = VERTEX_POINT ( 'NONE', #11961 ) ;
#10223 = CARTESIAN_POINT ( 'NONE',  ( 1.133692148550000001, -50.50000000000000000, -137.0552959530000123 ) ) ;
#10224 = CARTESIAN_POINT ( 'NONE',  ( 31.00000000000000000, 39.80430157320000006, -149.5552959529999839 ) ) ;
#10225 = VECTOR ( 'NONE', #1640, 1000.000000000000114 ) ;
#10226 = CARTESIAN_POINT ( 'NONE',  ( 24.28524365307783484, -17.57808196999505412, -150.0552959529999839 ) ) ;
#10227 = LINE ( 'NONE', #17498, #14442 ) ;
#10228 = LINE ( 'NONE', #1221, #14129 ) ;
#10229 = AXIS2_PLACEMENT_3D ( 'NONE', #2030, #11259, #9357 ) ;
#10230 = LINE ( 'NONE', #22734, #10183 ) ;
#10231 = EDGE_CURVE ( 'NONE', #10837, #18382, #4929, .T. ) ;
#10232 = ORIENTED_EDGE ( 'NONE', *, *, #3703, .F. ) ;
#10233 = CARTESIAN_POINT ( 'NONE',  ( -16.63107678134597833, 35.60580843634807735, -140.6802342587363910 ) ) ;
#10234 = PLANE ( 'NONE',  #8305 ) ;
#10235 = DIRECTION ( 'NONE',  ( 2.259525899719999991E-12, 0.000000000000000000, 1.000000000000000000 ) ) ;
#10236 = CARTESIAN_POINT ( 'NONE',  ( -4.521812268179999705, -27.38504028299999860, -148.0552959529999839 ) ) ;
#10237 = FACE_OUTER_BOUND ( 'NONE', #22376, .T. ) ;
#10238 = ORIENTED_EDGE ( 'NONE', *, *, #15416, .F. ) ;
#10239 = CARTESIAN_POINT ( 'NONE',  ( -9.592967682888913217, 35.51842212454483416, -147.1736941271391004 ) ) ;
#10240 = FACE_OUTER_BOUND ( 'NONE', #4934, .T. ) ;
#10241 = ADVANCED_FACE ( 'NONE', ( #15423 ), #8399, .T. ) ;
#10242 = CARTESIAN_POINT ( 'NONE',  ( 6.000000000000000000, -3.301262168631092564, -150.0552959530000123 ) ) ;
#10243 = EDGE_CURVE ( 'NONE', #19493, #1779, #8270, .T. ) ;
#10244 = VERTEX_POINT ( 'NONE', #13634 ) ;
#10245 = AXIS2_PLACEMENT_3D ( 'NONE', #3258, #5273, #21715 ) ;
#10246 = EDGE_CURVE ( 'NONE', #19589, #4360, #9935, .T. ) ;
#10247 = DIRECTION ( 'NONE',  ( -1.000000000000000000, 0.000000000000000000, 0.000000000000000000 ) ) ;
#10248 = AXIS2_PLACEMENT_3D ( 'NONE', #16407, #1785, #21885 ) ;
#10249 = VECTOR ( 'NONE', #10068, 1000.000000000000227 ) ;
#10250 = VECTOR ( 'NONE', #21416, 1000.000000000000114 ) ;
#10251 = CARTESIAN_POINT ( 'NONE',  ( -28.94327676059999988, 35.53474617860000251, -140.7339624629999832 ) ) ;
#10252 = DIRECTION ( 'NONE',  ( 0.000000000000000000, 1.603797727360000188E-26, -1.000000000000000000 ) ) ;
#10253 = EDGE_LOOP ( 'NONE', ( #8451, #10036, #9359, #11737, #21297, #10874 ) ) ;
#10254 = CARTESIAN_POINT ( 'NONE',  ( -23.96059125624836028, 40.27687008288653203, -142.1584808468900860 ) ) ;
#10255 = EDGE_CURVE ( 'NONE', #2559, #14557, #22032, .T. ) ;
#10256 = DIRECTION ( 'NONE',  ( -0.9954742291034677226, 0.09503188512734457583, 4.503363594322118746E-12 ) ) ;
#10257 = EDGE_CURVE ( 'NONE', #7545, #7540, #13512, .T. ) ;
#10258 = CARTESIAN_POINT ( 'NONE',  ( 25.50000000000000000, 25.50000000000000000, -151.0552959529999839 ) ) ;
#10259 = CARTESIAN_POINT ( 'NONE',  ( -12.87073128380000142, -34.50000000000000000, -149.4704070610000031 ) ) ;
#10260 = ORIENTED_EDGE ( 'NONE', *, *, #23166, .F. ) ;
#10261 = DIRECTION ( 'NONE',  ( 1.000000000000000000, 2.602084704489999637E-17, -2.257171095940000041E-12 ) ) ;
#10262 = EDGE_CURVE ( 'NONE', #9795, #21893, #4602, .T. ) ;
#10263 = CARTESIAN_POINT ( 'NONE',  ( 3.763193976707701172, -36.41260098204946871, -150.0552959530000123 ) ) ;
#10264 = CARTESIAN_POINT ( 'NONE',  ( 10.68320006080000084, -21.50000000000000000, -149.3052959529999839 ) ) ;
#10265 = ADVANCED_FACE ( 'NONE', ( #17207 ), #924, .F. ) ;
#10266 = ORIENTED_EDGE ( 'NONE', *, *, #12192, .F. ) ;
#10267 = CIRCLE ( 'NONE', #413, 3.499999999999999556 ) ;
#10268 = MECHANICAL_DESIGN_GEOMETRIC_PRESENTATION_REPRESENTATION (  '', ( #6857 ), #21305 ) ;
#10269 = CARTESIAN_POINT ( 'NONE',  ( -32.50000000000000000, 1.000000000000000000, -151.0552959529999839 ) ) ;
#10270 = EDGE_LOOP ( 'NONE', ( #12457, #11238, #1819, #3521 ) ) ;
#10271 = CARTESIAN_POINT ( 'NONE',  ( -7.724735339242877252, 33.29363753972616280, -144.6062484440719231 ) ) ;
#10272 = DIRECTION ( 'NONE',  ( 1.000000000000000000, 0.000000000000000000, -1.480297366166875808E-13 ) ) ;
#10273 = LINE ( 'NONE', #17297, #12695 ) ;
#10274 = ORIENTED_EDGE ( 'NONE', *, *, #14171, .F. ) ;
#10275 = FACE_OUTER_BOUND ( 'NONE', #5670, .T. ) ;
#10276 = CARTESIAN_POINT ( 'NONE',  ( -15.03885004549999849, 41.12207116019999376, -146.4108951270000034 ) ) ;
#10277 = ORIENTED_EDGE ( 'NONE', *, *, #19342, .F. ) ;
#10278 = CARTESIAN_POINT ( 'NONE',  ( -32.50000000000000000, 1.000000000000000000, -150.0552959529999839 ) ) ;
#10279 = CARTESIAN_POINT ( 'NONE',  ( -17.55745234318444759, 36.93608508457451478, -140.4812394866132763 ) ) ;
#10280 = CARTESIAN_POINT ( 'NONE',  ( -16.46164914215972885, -43.39061678754082862, -150.0552959530000123 ) ) ;
#10281 = CARTESIAN_POINT ( 'NONE',  ( 8.351115582570084683, -45.97632467507357035, -136.0552959530188559 ) ) ;
#10282 = MECHANICAL_DESIGN_GEOMETRIC_PRESENTATION_REPRESENTATION (  '', ( #11802 ), #20953 ) ;
#10283 = EDGE_CURVE ( 'NONE', #20361, #10772, #10048, .T. ) ;
#10284 = CARTESIAN_POINT ( 'NONE',  ( -24.60351133389204392, 36.30534674873651824, -147.3819557762199963 ) ) ;
#10285 = LINE ( 'NONE', #12065, #9365 ) ;
#10286 = CARTESIAN_POINT ( 'NONE',  ( -2.976504231241439591, 42.55205464666336468, -136.0552959530011776 ) ) ;
#10287 = EDGE_LOOP ( 'NONE', ( #17203, #2902, #18882, #8610 ) ) ;
#10288 = DIRECTION ( 'NONE',  ( 0.000000000000000000, 0.000000000000000000, 1.000000000000000000 ) ) ;
#10289 = ORIENTED_EDGE ( 'NONE', *, *, #4515, .F. ) ;
#10290 = ORIENTED_EDGE ( 'NONE', *, *, #4133, .F. ) ;
#10291 = ORIENTED_EDGE ( 'NONE', *, *, #177, .F. ) ;
#10292 = CARTESIAN_POINT ( 'NONE',  ( -0.7601318171273256930, 22.44600007524324781, -136.0552959529983070 ) ) ;
#10293 = CARTESIAN_POINT ( 'NONE',  ( 5.749999999879999102, -3.000000000000000000, -135.4552959529999896 ) ) ;
#10294 = ORIENTED_EDGE ( 'NONE', *, *, #12849, .T. ) ;
#10295 = AXIS2_PLACEMENT_3D ( 'NONE', #10313, #22947, #6630 ) ;
#10296 = VECTOR ( 'NONE', #2421, 1000.000000000000000 ) ;
#10297 = ORIENTED_EDGE ( 'NONE', *, *, #5415, .T. ) ;
#10298 = DIRECTION ( 'NONE',  ( -0.07970438983373200059, -0.9968185442904001770, 8.268133652483321323E-13 ) ) ;
#10299 = CARTESIAN_POINT ( 'NONE',  ( -19.28609856419999957, 34.66429844339999988, -140.9609051179999994 ) ) ;
#10300 = CARTESIAN_POINT ( 'NONE',  ( -11.11377970773875923, 36.98904460433606545, -140.6889018750556772 ) ) ;
#10301 = FILL_AREA_STYLE ('',( #13515 ) ) ;
#10302 = CARTESIAN_POINT ( 'NONE',  ( -7.687380149402162743, 32.47466110599622624, -144.7109350977037820 ) ) ;
#10303 = CARTESIAN_POINT ( 'NONE',  ( -9.624908808166578567, 40.88242544008282664, -146.1844385046725279 ) ) ;
#10304 = VERTEX_POINT ( 'NONE', #17325 ) ;
#10305 = CARTESIAN_POINT ( 'NONE',  ( -28.70612892850000009, 35.15950212979999634, -139.8035036599999898 ) ) ;
#10306 = EDGE_CURVE ( 'NONE', #11337, #8510, #3411, .T. ) ;
#10307 = CARTESIAN_POINT ( 'NONE',  ( -7.529689113779999943, 37.05876528330000497, -139.9906690790000141 ) ) ;
#10308 = DIRECTION ( 'NONE',  ( 0.000000000000000000, -1.000000000000000000, -2.765629237170000203E-27 ) ) ;
#10309 = AXIS2_PLACEMENT_3D ( 'NONE', #13337, #9399, #11078 ) ;
#10310 = VERTEX_POINT ( 'NONE', #18041 ) ;
#10311 = AXIS2_PLACEMENT_3D ( 'NONE', #7055, #49, #16225 ) ;
#10312 = B_SPLINE_CURVE_WITH_KNOTS ( 'NONE', 5,
 ( #330, #20214, #1582, #9346, #21558, #5241, #4896, #10462, #19646, #3122, #5680, #20088 ),
 .UNSPECIFIED., .F., .F.,
 ( 6, 3, 3, 6 ),
 ( 0.000000000000000000, 4.509114667229999540, 8.972055907920001516, 13.39149027789999913 ),
 .UNSPECIFIED. ) ;
#10313 = CARTESIAN_POINT ( 'NONE',  ( -4.959431410700000598, -23.66636161550000139, -145.5552959529999839 ) ) ;
#10314 = ORIENTED_EDGE ( 'NONE', *, *, #952, .F. ) ;
#10315 = DIRECTION ( 'NONE',  ( 0.000000000000000000, -1.000000000000000000, 0.000000000000000000 ) ) ;
#10316 = DIRECTION ( 'NONE',  ( -0.6459422414661291079, -0.7633862853691523176, -2.273736754430455399E-12 ) ) ;
#10317 = ORIENTED_EDGE ( 'NONE', *, *, #6974, .F. ) ;
#10318 = DIRECTION ( 'NONE',  ( -1.000000000000000000, -3.994014902950000436E-29, 0.000000000000000000 ) ) ;
#10319 = DIRECTION ( 'NONE',  ( 0.000000000000000000, 1.000000000000000000, 0.000000000000000000 ) ) ;
#10320 = ORIENTED_EDGE ( 'NONE', *, *, #633, .T. ) ;
#10321 = CARTESIAN_POINT ( 'NONE',  ( -15.00140173380579967, 40.20535686067439940, -145.8913236318788051 ) ) ;
#10322 = CARTESIAN_POINT ( 'NONE',  ( -25.81549887252723252, 32.87029380595873818, -144.5911656381801151 ) ) ;
#10323 = ORIENTED_EDGE ( 'NONE', *, *, #10255, .T. ) ;
#10324 = ORIENTED_EDGE ( 'NONE', *, *, #19122, .F. ) ;
#10325 = CARTESIAN_POINT ( 'NONE',  ( -21.35824191589999899, -4.000000000000000000, -144.8157682190000060 ) ) ;
#10326 = DIRECTION ( 'NONE',  ( 0.000000000000000000, -0.4794255386042052813, -0.8775825618903714265 ) ) ;
#10327 = ORIENTED_EDGE ( 'NONE', *, *, #8716, .F. ) ;
#10328 = VECTOR ( 'NONE', #10319, 1000.000000000000000 ) ;
#10329 = FACE_OUTER_BOUND ( 'NONE', #17115, .T. ) ;
#10330 = AXIS2_PLACEMENT_3D ( 'NONE', #5267, #12521, #23476 ) ;
#10331 = VECTOR ( 'NONE', #5342, 1000.000000000000000 ) ;
#10332 = CARTESIAN_POINT ( 'NONE',  ( -35.47299999999999898, 16.95803989150000035, -143.5552959529999839 ) ) ;
#10333 = CARTESIAN_POINT ( 'NONE',  ( -35.47299999999999898, 16.63274768570000006, -142.6170193369999879 ) ) ;
#10334 = EDGE_CURVE ( 'NONE', #5071, #20358, #15892, .T. ) ;
#10335 = EDGE_CURVE ( 'NONE', #8887, #15850, #5293, .T. ) ;
#10336 = ORIENTED_EDGE ( 'NONE', *, *, #12192, .T. ) ;
#10337 = CARTESIAN_POINT ( 'NONE',  ( 19.91945158500000090, 51.14507942810000429, -150.0552959519999945 ) ) ;
#10338 = DIRECTION ( 'NONE',  ( 1.000000000000000000, 0.000000000000000000, 0.000000000000000000 ) ) ;
#10339 = CARTESIAN_POINT ( 'NONE',  ( -15.36599175860845889, 37.73046438850320072, -147.5598381917453992 ) ) ;
#10340 = CARTESIAN_POINT ( 'NONE',  ( -28.93111463330243893, 37.94265998448511823, -140.6213208041744736 ) ) ;
#10341 = ORIENTED_EDGE ( 'NONE', *, *, #4458, .F. ) ;
#10342 = DIRECTION ( 'NONE',  ( 1.000000000000000000, 0.000000000000000000, 0.000000000000000000 ) ) ;
#10343 = CIRCLE ( 'NONE', #13003, 1.000000000000000888 ) ;
#10344 = DIRECTION ( 'NONE',  ( -1.000000000000000000, 0.000000000000000000, 0.000000000000000000 ) ) ;
#10345 = DIRECTION ( 'NONE',  ( 0.000000000000000000, 0.000000000000000000, -1.000000000000000000 ) ) ;
#10346 = CARTESIAN_POINT ( 'NONE',  ( 13.98502865247636961, 39.11890206003843673, -136.0552959530315889 ) ) ;
#10347 = CARTESIAN_POINT ( 'NONE',  ( -22.10824191591069265, -32.00000000000000000, -141.9623572383543717 ) ) ;
#10348 = ORIENTED_EDGE ( 'NONE', *, *, #15586, .T. ) ;
#10349 = EDGE_CURVE ( 'NONE', #16889, #13555, #11001, .T. ) ;
#10350 = CARTESIAN_POINT ( 'NONE',  ( -16.04375348400463608, 33.06607696223074555, -141.5117709027480259 ) ) ;
#10351 = DIRECTION ( 'NONE',  ( -0.000000000000000000, 1.000000000000000000, 0.000000000000000000 ) ) ;
#10352 = DIRECTION ( 'NONE',  ( 0.000000000000000000, 1.000000000000000000, 0.000000000000000000 ) ) ;
#10353 = CARTESIAN_POINT ( 'NONE',  ( -26.47299999999999898, 15.75516512379999945, -143.0964448760000209 ) ) ;
#10354 = DIRECTION ( 'NONE',  ( -0.09606172499277226828, -0.9953753789357124848, 8.268372250837614805E-13 ) ) ;
#10355 = EDGE_CURVE ( 'NONE', #1242, #11614, #9845, .T. ) ;
#10356 = ORIENTED_EDGE ( 'NONE', *, *, #17254, .T. ) ;
#10357 = FACE_OUTER_BOUND ( 'NONE', #14441, .T. ) ;
#10358 = LINE ( 'NONE', #15964, #2988 ) ;
#10359 = EDGE_LOOP ( 'NONE', ( #10516, #22583, #3425, #16438 ) ) ;
#10360 = CARTESIAN_POINT ( 'NONE',  ( -29.19553354363359077, 36.02155055457190969, -139.4833455107854832 ) ) ;
#10361 = EDGE_CURVE ( 'NONE', #6401, #21499, #19942, .T. ) ;
#10362 = PLANE ( 'NONE',  #19738 ) ;
#10363 = VERTEX_POINT ( 'NONE', #8974 ) ;
#10364 = CARTESIAN_POINT ( 'NONE',  ( 29.68320006080000084, -24.50000000000000000, -149.3052959529999839 ) ) ;
#10365 = DIRECTION ( 'NONE',  ( -1.000000000000000000, 0.000000000000000000, 0.000000000000000000 ) ) ;
#10366 = DIRECTION ( 'NONE',  ( 0.000000000000000000, 0.000000000000000000, 1.000000000000000000 ) ) ;
#10367 = LINE ( 'NONE', #6460, #10586 ) ;
#10368 = ORIENTED_EDGE ( 'NONE', *, *, #6162, .T. ) ;
#10369 = CARTESIAN_POINT ( 'NONE',  ( -10.75335342199438671, 32.39647868472179937, -144.3483278521977411 ) ) ;
#10370 = CARTESIAN_POINT ( 'NONE',  ( -18.85469010170000459, 37.03971195569999963, -148.4264296979999926 ) ) ;
#10371 = CARTESIAN_POINT ( 'NONE',  ( -8.730967964694192673, 38.58574671193542827, -147.7727093204715914 ) ) ;
#10372 = LINE ( 'NONE', #8582, #845 ) ;
#10373 = ADVANCED_FACE ( 'NONE', ( #18281 ), #19830, .F. ) ;
#10374 = ORIENTED_EDGE ( 'NONE', *, *, #1847, .T. ) ;
#10375 = AXIS2_PLACEMENT_3D ( 'NONE', #10431, #23418, #5336 ) ;
#10376 = ORIENTED_EDGE ( 'NONE', *, *, #19383, .T. ) ;
#10377 = CARTESIAN_POINT ( 'NONE',  ( -6.804059094871798052, 37.03366832437883716, -147.4295713064250890 ) ) ;
#10378 = CARTESIAN_POINT ( 'NONE',  ( -29.18503926089999823, 39.40432144729999919, -139.9690405629999930 ) ) ;
#10379 = CARTESIAN_POINT ( 'NONE',  ( -21.90852802850000103, 37.90475843469999973, -148.1502781210000137 ) ) ;
#10380 = EDGE_CURVE ( 'NONE', #4187, #11626, #5181, .T. ) ;
#10381 = ORIENTED_EDGE ( 'NONE', *, *, #5376, .T. ) ;
#10382 = DIRECTION ( 'NONE',  ( -2.257171095940000041E-12, 7.494005416210000121E-16, -1.000000000000000000 ) ) ;
#10383 = DIRECTION ( 'NONE',  ( 1.527666881879999979E-13, 8.153477892850000134E-13, 1.000000000000000000 ) ) ;
#10384 = ADVANCED_FACE ( 'NONE', ( #8861 ), #5303, .T. ) ;
#10385 = ORIENTED_EDGE ( 'NONE', *, *, #10306, .T. ) ;
#10386 = CARTESIAN_POINT ( 'NONE',  ( -21.70512920578378058, 38.46301180794304031, -147.3000385647142139 ) ) ;
#10387 = ADVANCED_FACE ( 'NONE', ( #10877 ), #23512, .F. ) ;
#10388 = EDGE_CURVE ( 'NONE', #18640, #3680, #15754, .T. ) ;
#10389 = CYLINDRICAL_SURFACE ( 'NONE', #1524, 10.00000000000000178 ) ;
#10390 = CARTESIAN_POINT ( 'NONE',  ( 7.683200060759999950, -20.50000000000000000, -138.5552959529999839 ) ) ;
#10391 = CARTESIAN_POINT ( 'NONE',  ( 5.004065293357752964, -45.75992235983020606, -136.0552959530113242 ) ) ;
#10392 = DIRECTION ( 'NONE',  ( 1.000000000000000000, 0.000000000000000000, 0.000000000000000000 ) ) ;
#10393 = AXIS2_PLACEMENT_3D ( 'NONE', #2738, #13427, #13666 ) ;
#10394 = CARTESIAN_POINT ( 'NONE',  ( -16.71251657190000017, 33.01037093000000766, -141.5651630139999781 ) ) ;
#10395 = CARTESIAN_POINT ( 'NONE',  ( 8.212854026800000540, -28.22404483660000096, -144.5552959529999839 ) ) ;
#10396 = CARTESIAN_POINT ( 'NONE',  ( -34.50000000000000000, 14.00000000000000000, -144.0552959529999839 ) ) ;
#10397 = VERTEX_POINT ( 'NONE', #10517 ) ;
#10398 = CARTESIAN_POINT ( 'NONE',  ( -23.32853373970706912, 36.96341023006314686, -139.4571126576171878 ) ) ;
#10399 = UNCERTAINTY_MEASURE_WITH_UNIT (LENGTH_MEASURE( 1.000000000000000082E-05 ), #6218, 'distance_accuracy_value', 'NONE');
#10400 = ORIENTED_EDGE ( 'NONE', *, *, #6628, .T. ) ;
#10401 =( LENGTH_UNIT ( ) NAMED_UNIT ( * ) SI_UNIT ( .MILLI., .METRE. ) );
#10402 = ORIENTED_EDGE ( 'NONE', *, *, #18549, .T. ) ;
#10403 = DIRECTION ( 'NONE',  ( 0.000000000000000000, -1.000000000000000000, -1.723073263340000007E-12 ) ) ;
#10404 = DIRECTION ( 'NONE',  ( 1.526468026909999897E-13, 8.159623473500000156E-13, 1.000000000000000000 ) ) ;
#10405 = ORIENTED_EDGE ( 'NONE', *, *, #4708, .T. ) ;
#10406 = EDGE_CURVE ( 'NONE', #21462, #9003, #5429, .T. ) ;
#10407 = ORIENTED_EDGE ( 'NONE', *, *, #9605, .T. ) ;
#10408 = CIRCLE ( 'NONE', #8116, 9.999999999999998224 ) ;
#10409 = CARTESIAN_POINT ( 'NONE',  ( 32.50000000000000000, 26.96379895119999759, -137.0552959530000123 ) ) ;
#10410 = CARTESIAN_POINT ( 'NONE',  ( -18.82091118379999983, 33.23810407359999886, -144.5979112940000277 ) ) ;
#10411 = EDGE_CURVE ( 'NONE', #2271, #7733, #20014, .T. ) ;
#10412 = CARTESIAN_POINT ( 'NONE',  ( -11.69335150359915687, 39.46909266604216526, -147.6919637091589550 ) ) ;
#10413 = CARTESIAN_POINT ( 'NONE',  ( -30.49999999990000177, 29.00000000000000000, -140.5552959529999839 ) ) ;
#10414 = CARTESIAN_POINT ( 'NONE',  ( -7.706057744140959898, 32.88414932316476325, -144.6585917708268028 ) ) ;
#10415 = ORIENTED_EDGE ( 'NONE', *, *, #17078, .F. ) ;
#10416 = CYLINDRICAL_SURFACE ( 'NONE', #13245, 5.000000000000000888 ) ;
#10417 = CARTESIAN_POINT ( 'NONE',  ( 6.000000000050000004, 37.00000000000000000, -149.5552959529999839 ) ) ;
#10418 = DIRECTION ( 'NONE',  ( 1.000000000000000000, 0.000000000000000000, 0.000000000000000000 ) ) ;
#10419 = ORIENTED_EDGE ( 'NONE', *, *, #2016, .T. ) ;
#10420 = CARTESIAN_POINT ( 'NONE',  ( -21.35824191589999899, -4.000000000000000000, -144.8157682190000060 ) ) ;
#10421 = ORIENTED_EDGE ( 'NONE', *, *, #9190, .T. ) ;
#10422 = DIRECTION ( 'NONE',  ( 0.000000000000000000, 0.000000000000000000, 1.000000000000000000 ) ) ;
#10423 = DIRECTION ( 'NONE',  ( 0.000000000000000000, -1.000000000000000000, 0.000000000000000000 ) ) ;
#10424 = ORIENTED_EDGE ( 'NONE', *, *, #16680, .F. ) ;
#10425 = CARTESIAN_POINT ( 'NONE',  ( 10.00000000010000001, 37.00000000000000000, -146.5552959529999839 ) ) ;
#10426 = CARTESIAN_POINT ( 'NONE',  ( -10.76224745929999926, 37.97907322949999553, -139.7231730900000173 ) ) ;
#10427 = VERTEX_POINT ( 'NONE', #22427 ) ;
#10428 = CARTESIAN_POINT ( 'NONE',  ( -21.03694116389347712, 36.94210036640072303, -147.9486865818473973 ) ) ;
#10429 = CARTESIAN_POINT ( 'NONE',  ( -25.64408091310000160, 33.16124342930000068, -144.5387451670000019 ) ) ;
#10430 = ORIENTED_EDGE ( 'NONE', *, *, #374, .T. ) ;
#10431 = CARTESIAN_POINT ( 'NONE',  ( 0.000000000000000000, 0.000000000000000000, 0.000000000000000000 ) ) ;
#10432 = EDGE_CURVE ( 'NONE', #6865, #4983, #14935, .T. ) ;
#10433 = ORIENTED_EDGE ( 'NONE', *, *, #3440, .T. ) ;
#10434 = CARTESIAN_POINT ( 'NONE',  ( -12.48399912370000031, 39.13586957980000136, -147.0556079069999953 ) ) ;
#10435 = EDGE_CURVE ( 'NONE', #19654, #19967, #13139, .T. ) ;
#10436 = DIRECTION ( 'NONE',  ( 8.955190032050000935E-12, -9.104778821549999739E-13, 1.000000000000000000 ) ) ;
#10437 = VERTEX_POINT ( 'NONE', #20528 ) ;
#10438 = FACE_OUTER_BOUND ( 'NONE', #1417, .T. ) ;
#10439 = CARTESIAN_POINT ( 'NONE',  ( 12.81474735470000148, -17.96536370379999781, -143.5552959529999839 ) ) ;
#10440 = ORIENTED_EDGE ( 'NONE', *, *, #15196, .T. ) ;
#10441 = DIRECTION ( 'NONE',  ( 1.000000000000000000, 0.000000000000000000, -2.257453483404482811E-12 ) ) ;
#10442 = CIRCLE ( 'NONE', #10814, 2.000000000000000000 ) ;
#10443 = ORIENTED_EDGE ( 'NONE', *, *, #9433, .T. ) ;
#10444 = CARTESIAN_POINT ( 'NONE',  ( 31.50000000000000000, 20.96379895120000114, -136.5552959530000123 ) ) ;
#10445 = DIRECTION ( 'NONE',  ( 5.094701932209999624E-24, 1.000000000000000000, -1.149947916579999802E-35 ) ) ;
#10446 = CARTESIAN_POINT ( 'NONE',  ( -14.16161598212295125, 40.91800955835415721, -144.5270132969140207 ) ) ;
#10447 = CARTESIAN_POINT ( 'NONE',  ( 8.500000000050000892, 37.00000000000000000, -148.7552959530000010 ) ) ;
#10448 = VERTEX_POINT ( 'NONE', #22305 ) ;
#10449 = LINE ( 'NONE', #4765, #16940 ) ;
#10450 = CARTESIAN_POINT ( 'NONE',  ( 6.500000000130000011, 20.50000000000000000, -150.5552959529999839 ) ) ;
#10451 = PLANE ( 'NONE',  #18985 ) ;
#10452 = CARTESIAN_POINT ( 'NONE',  ( 22.33963087269999903, -30.94765732060000119, -147.5552959529999839 ) ) ;
#10453 = DIRECTION ( 'NONE',  ( -0.7071067811866730279, 0.6205445805637129775, 0.3390050494208429743 ) ) ;
#10454 = VECTOR ( 'NONE', #5956, 1000.000000000000000 ) ;
#10455 = VECTOR ( 'NONE', #8721, 1000.000000000000000 ) ;
#10456 = VERTEX_POINT ( 'NONE', #22081 ) ;
#10457 = LINE ( 'NONE', #19641, #7646 ) ;
#10458 = DIRECTION ( 'NONE',  ( -0.9896415801065049367, 0.1435602414469282218, 8.993136838065500309E-12 ) ) ;
#10459 = EDGE_CURVE ( 'NONE', #10616, #5898, #304, .T. ) ;
#10460 = CARTESIAN_POINT ( 'NONE',  ( 31.82297112100000192, -40.41789419119999849, -150.0552959529999839 ) ) ;
#10461 = CARTESIAN_POINT ( 'NONE',  ( -5.271986118780953134, 36.97016010513711848, -139.4665544805324089 ) ) ;
#10462 = CARTESIAN_POINT ( 'NONE',  ( -24.49703822390000241, 40.50511125069999707, -146.0729279460000214 ) ) ;
#10463 = EDGE_CURVE ( 'NONE', #16855, #8795, #16947, .T. ) ;
#10464 = DIRECTION ( 'NONE',  ( 1.000000000000000000, 0.000000000000000000, -2.257120985840000117E-12 ) ) ;
#10465 = ORIENTED_EDGE ( 'NONE', *, *, #10111, .F. ) ;
#10466 = FACE_OUTER_BOUND ( 'NONE', #20637, .T. ) ;
#10467 = DIRECTION ( 'NONE',  ( -0.000000000000000000, 1.000000000000000000, 0.000000000000000000 ) ) ;
#10468 = VERTEX_POINT ( 'NONE', #9671 ) ;
#10470 = CARTESIAN_POINT ( 'NONE',  ( -28.99748895112272251, 32.89468467962849729, -143.6350524796266654 ) ) ;
#10469 = VECTOR ( 'NONE', #10774, 1000.000000000000000 ) ;
#10471 = AXIS2_PLACEMENT_3D ( 'NONE', #12857, #12980, #16210 ) ;
#10472 = CARTESIAN_POINT ( 'NONE',  ( -18.35824191589999899, -13.50000000000000000, -146.3157682190000060 ) ) ;
#10473 = VERTEX_POINT ( 'NONE', #5998 ) ;
#10474 = DIRECTION ( 'NONE',  ( 0.000000000000000000, 1.000000000000000000, 0.000000000000000000 ) ) ;
#10475 = PLANE ( 'NONE',  #13147 ) ;
#10476 = CARTESIAN_POINT ( 'NONE',  ( 4.999999999879999990, -5.500000000000000000, -135.4552959529999896 ) ) ;
#10477 = CARTESIAN_POINT ( 'NONE',  ( 7.702812687520848911, 38.27075047946028974, -141.9023098454317449 ) ) ;
#10478 = VERTEX_POINT ( 'NONE', #14695 ) ;
#10479 = DIRECTION ( 'NONE',  ( -0.9753087663813413410, 0.2208456705930775810, 0.000000000000000000 ) ) ;
#10480 = CARTESIAN_POINT ( 'NONE',  ( -8.151404454119415277, 40.91889870648304139, -143.6674959883383167 ) ) ;
#10481 = CARTESIAN_POINT ( 'NONE',  ( 9.444192711154135722, -32.39608312526165435, -136.0552959530213002 ) ) ;
#10482 = EDGE_CURVE ( 'NONE', #17961, #34, #1922, .T. ) ;
#10483 = VERTEX_POINT ( 'NONE', #21964 ) ;
#10484 = CARTESIAN_POINT ( 'NONE',  ( -20.60824191589185972, -4.000000000000000000, -149.4708568729739966 ) ) ;
#10485 = ORIENTED_EDGE ( 'NONE', *, *, #11887, .T. ) ;
#10486 = VECTOR ( 'NONE', #17423, 1000.000000000000114 ) ;
#10487 = CARTESIAN_POINT ( 'NONE',  ( -7.529689113779999943, 37.05876528330000497, -139.9906690790000141 ) ) ;
#10488 = DIRECTION ( 'NONE',  ( -0.07970438983373200059, -0.9968185442904001770, 8.242295734823311485E-13 ) ) ;
#10489 = EDGE_CURVE ( 'NONE', #15926, #12978, #14823, .T. ) ;
#10490 = CARTESIAN_POINT ( 'NONE',  ( 11.68320006080000262, -20.76179938779915446, -148.5552959529999839 ) ) ;
#10491 = ORIENTED_EDGE ( 'NONE', *, *, #2860, .F. ) ;
#10492 = LINE ( 'NONE', #1488, #14828 ) ;
#10493 = ORIENTED_EDGE ( 'NONE', *, *, #391, .F. ) ;
#10494 = CARTESIAN_POINT ( 'NONE',  ( -7.816799939239999162, -1.500000000000000000, -150.0552959529999839 ) ) ;
#10495 = CARTESIAN_POINT ( 'NONE',  ( -9.157754307290000284, -15.75963164970000108, -147.5552959529999839 ) ) ;
#10496 = CARTESIAN_POINT ( 'NONE',  ( -12.60099947280546218, -41.15635984007524684, -150.0552959529999839 ) ) ;
#10497 = CARTESIAN_POINT ( 'NONE',  ( 31.50000000010000178, -33.03620104880000241, -136.0552959530000123 ) ) ;
#10498 = AXIS2_PLACEMENT_3D ( 'NONE', #4559, #22531, #9770 ) ;
#10499 = DIRECTION ( 'NONE',  ( 1.000000000000000000, 0.000000000000000000, -4.510774274160000731E-12 ) ) ;
#10500 = CIRCLE ( 'NONE', #13554, 1.499999999999999556 ) ;
#10501 = CARTESIAN_POINT ( 'NONE',  ( -17.13033207850000039, 36.08498863180000171, -139.6042211940000186 ) ) ;
#10502 = SHAPE_DEFINITION_REPRESENTATION ( #21844, #3728 ) ;
#10503 = DIRECTION ( 'NONE',  ( -0.9953753789357124848, 0.09606172499277215726, 7.216449660063520037E-14 ) ) ;
#10504 = CARTESIAN_POINT ( 'NONE',  ( -3.499999999929999994, 31.50000000000000000, -138.0552959530000123 ) ) ;
#10505 = EDGE_CURVE ( 'NONE', #19799, #10172, #18624, .T. ) ;
#10506 = ORIENTED_EDGE ( 'NONE', *, *, #13645, .F. ) ;
#10507 = CYLINDRICAL_SURFACE ( 'NONE', #3354, 7.500000000000006217 ) ;
#10508 =( BOUNDED_CURVE ( )  B_SPLINE_CURVE ( 5, ( #13731, #8005, #10378, #4691, #6585, #21231, #2908, #6700, #17538 ),
 .UNSPECIFIED., .F., .F. ) 
 B_SPLINE_CURVE_WITH_KNOTS ( ( 6, 3, 6 ),
 ( 0.000000000000000000, 5.731822293570000504, 9.005131590149998644 ),
 .UNSPECIFIED. ) 
 CURVE ( )  GEOMETRIC_REPRESENTATION_ITEM ( )  RATIONAL_B_SPLINE_CURVE ( ( 0.2500000000000000000, 0.2500000000000000000, 0.2500000000000000000, 0.2500000000000000000, 0.2500000000000000000, 0.2500000000000000000, 0.2500000000000000000, 0.2500000000000000000, 0.2500000000000000000 ) ) 
 REPRESENTATION_ITEM ( '' )  );
#10509 = ADVANCED_FACE ( 'NONE', ( #11339 ), #4340, .T. ) ;
#10510 = ORIENTED_EDGE ( 'NONE', *, *, #14548, .F. ) ;
#10511 = ORIENTED_EDGE ( 'NONE', *, *, #20346, .T. ) ;
#10512 = CARTESIAN_POINT ( 'NONE',  ( 32.05742780190000474, 40.87448416769999682, -149.5552959529999839 ) ) ;
#10513 = LINE ( 'NONE', #19824, #13341 ) ;
#10514 = LINE ( 'NONE', #17795, #3098 ) ;
#10515 = VECTOR ( 'NONE', #20258, 1000.000000000000000 ) ;
#10516 = ORIENTED_EDGE ( 'NONE', *, *, #7770, .F. ) ;
#10517 = CARTESIAN_POINT ( 'NONE',  ( -19.59255166829999695, 37.05126161860000167, -140.3061871179999969 ) ) ;
#10518 = CARTESIAN_POINT ( 'NONE',  ( -9.292483939630001188, 40.96918990780000058, -144.3907905730000039 ) ) ;
#10519 = AXIS2_PLACEMENT_3D ( 'NONE', #2323, #15150, #20283 ) ;
#10520 = DIRECTION ( 'NONE',  ( 0.000000000000000000, -1.000000000000000000, 0.000000000000000000 ) ) ;
#10521 = CARTESIAN_POINT ( 'NONE',  ( -32.50000000000000000, -74.00000000000000000, -144.0552959529999839 ) ) ;
#10522 = ORIENTED_EDGE ( 'NONE', *, *, #21099, .T. ) ;
#10523 = DIRECTION ( 'NONE',  ( 1.000000000000000000, 0.000000000000000000, -2.257144641399999941E-12 ) ) ;
#10524 = ORIENTED_EDGE ( 'NONE', *, *, #23486, .F. ) ;
#10525 = EDGE_CURVE ( 'NONE', #2277, #17363, #7888, .T. ) ;
#10526 = CARTESIAN_POINT ( 'NONE',  ( 9.848540439720265383, 36.34242854357029984, -141.6431750412639303 ) ) ;
#10527 = ADVANCED_FACE ( 'NONE', ( #12906 ), #20187, .F. ) ;
#10528 = CARTESIAN_POINT ( 'NONE',  ( -32.50000000000000000, 67.50000000000000000, -144.0552959529999839 ) ) ;
#10529 = DIRECTION ( 'NONE',  ( -2.602084704489999637E-17, 1.000000000000000000, 0.000000000000000000 ) ) ;
#10530 = EDGE_LOOP ( 'NONE', ( #1918, #3903, #5946, #13935 ) ) ;
#10531 = AXIS2_PLACEMENT_3D ( 'NONE', #21432, #19409, #6781 ) ;
#10532 = EDGE_CURVE ( 'NONE', #19961, #18313, #400, .T. ) ;
#10533 = EDGE_CURVE ( 'NONE', #11647, #1347, #11222, .T. ) ;
#10534 = CARTESIAN_POINT ( 'NONE',  ( 0.5000000001500000124, 24.10555127549999810, -143.5552959529999839 ) ) ;
#10535 = VECTOR ( 'NONE', #21428, 1000.000000000000000 ) ;
#10536 = ORIENTED_EDGE ( 'NONE', *, *, #14317, .F. ) ;
#10537 = DIRECTION ( 'NONE',  ( 0.000000000000000000, 1.000000000000000000, 2.257144641399999941E-12 ) ) ;
#10538 = CARTESIAN_POINT ( 'NONE',  ( -34.50000000000000000, 14.00000000000000000, -144.0552959529999839 ) ) ;
#10539 = EDGE_CURVE ( 'NONE', #12475, #20935, #2214, .T. ) ;
#10540 = ORIENTED_EDGE ( 'NONE', *, *, #1797, .F. ) ;
#10541 = CARTESIAN_POINT ( 'NONE',  ( -9.334216945200001447, -17.19633444960000190, -146.5552959529999839 ) ) ;
#10542 = ORIENTED_EDGE ( 'NONE', *, *, #16018, .F. ) ;
#10543 = CARTESIAN_POINT ( 'NONE',  ( -15.39869693353375268, 40.21355843083121329, -145.8451804845391280 ) ) ;
#10544 = ADVANCED_FACE ( 'NONE', ( #426 ), #21002, .F. ) ;
#10545 = CARTESIAN_POINT ( 'NONE',  ( -5.246332636038733455, 43.48990303080123709, -150.0552959529999839 ) ) ;
#10546 = VERTEX_POINT ( 'NONE', #15516 ) ;
#10547 = FILL_AREA_STYLE ('',( #18181 ) ) ;
#10548 = ORIENTED_EDGE ( 'NONE', *, *, #11919, .T. ) ;
#10549 = CARTESIAN_POINT ( 'NONE',  ( -25.64792992843672081, 37.04465132569895758, -139.7265440088568198 ) ) ;
#10550 = DIRECTION ( 'NONE',  ( 0.000000000000000000, 0.000000000000000000, 1.000000000000000000 ) ) ;
#10551 = ORIENTED_EDGE ( 'NONE', *, *, #7072, .F. ) ;
#10552 = CARTESIAN_POINT ( 'NONE',  ( 23.50000000000000000, -20.50000000000000000, -137.0552959530000123 ) ) ;
#10553 = AXIS2_PLACEMENT_3D ( 'NONE', #5772, #308, #1997 ) ;
#10554 = LINE ( 'NONE', #10909, #17044 ) ;
#10555 = ORIENTED_EDGE ( 'NONE', *, *, #21836, .F. ) ;
#10556 = VECTOR ( 'NONE', #10288, 1000.000000000000000 ) ;
#10557 = CARTESIAN_POINT ( 'NONE',  ( 20.50000000000000000, 19.50000000000000000, -151.0552959529999839 ) ) ;
#10558 = ORIENTED_EDGE ( 'NONE', *, *, #18855, .F. ) ;
#10559 = CARTESIAN_POINT ( 'NONE',  ( -18.07392865170000107, -1.500000000000000000, -144.8157682190000060 ) ) ;
#10560 = CYLINDRICAL_SURFACE ( 'NONE', #1352, 3.499999999999999556 ) ;
#10561 = ADVANCED_FACE ( 'NONE', ( #17542 ), #19091, .F. ) ;
#10562 = CARTESIAN_POINT ( 'NONE',  ( -14.58162373624594110, 40.18882273015199758, -142.1871799654946074 ) ) ;
#10563 = DIRECTION ( 'NONE',  ( 1.000000000000000000, 0.000000000000000000, 2.516505522483685870E-12 ) ) ;
#10564 = ORIENTED_EDGE ( 'NONE', *, *, #907, .F. ) ;
#10565 = CARTESIAN_POINT ( 'NONE',  ( -15.53720866509999965, -34.50000000000000000, -147.3052959529999839 ) ) ;
#10566 = AXIS2_PLACEMENT_3D ( 'NONE', #9355, #16626, #4026 ) ;
#10567 = CARTESIAN_POINT ( 'NONE',  ( 29.68320006080000084, -32.50000000000000000, -150.0552959529999839 ) ) ;
#10568 = LINE ( 'NONE', #8552, #22795 ) ;
#10569 = CARTESIAN_POINT ( 'NONE',  ( -30.49999999990000177, 37.00000000000000000, -144.0552959529999839 ) ) ;
#10570 = CARTESIAN_POINT ( 'NONE',  ( 6.000000000160000013, 36.50000000000000000, -139.5552959529999839 ) ) ;
#10571 = VECTOR ( 'NONE', #14282, 1000.000000000000000 ) ;
#10572 = ORIENTED_EDGE ( 'NONE', *, *, #14864, .F. ) ;
#10573 = CARTESIAN_POINT ( 'NONE',  ( 0.8371776177479999248, 16.00000000000000000, -144.0552959529999839 ) ) ;
#10574 = AXIS2_PLACEMENT_3D ( 'NONE', #7569, #18517, #2236 ) ;
#10575 = PLANE ( 'NONE',  #1563 ) ;
#10576 = VECTOR ( 'NONE', #18913, 1000.000000000000000 ) ;
#10577 = DIRECTION ( 'NONE',  ( 1.000000000000000000, 0.000000000000000000, -1.522591576628786004E-13 ) ) ;
#10578 = CARTESIAN_POINT ( 'NONE',  ( -5.974012367534657031, 36.93458879463069167, -148.2930816546209769 ) ) ;
#10579 = CARTESIAN_POINT ( 'NONE',  ( -9.056357402059999728, -12.43025388040000045, -147.5552959529999839 ) ) ;
#10580 = CARTESIAN_POINT ( 'NONE',  ( 19.68320006079999729, -16.50000000000000000, -149.3052959529999839 ) ) ;
#10581 = ORIENTED_EDGE ( 'NONE', *, *, #19294, .T. ) ;
#10582 = DIRECTION ( 'NONE',  ( 1.000000000000000000, 0.000000000000000000, 0.000000000000000000 ) ) ;
#10583 = DIRECTION ( 'NONE',  ( 1.000000000000000000, 2.602084704489999637E-17, -1.701177084830000066E-20 ) ) ;
#10584 = ORIENTED_EDGE ( 'NONE', *, *, #5032, .F. ) ;
#10585 = VECTOR ( 'NONE', #14729, 1000.000000000000000 ) ;
#10586 = VECTOR ( 'NONE', #21221, 1000.000000000000114 ) ;
#10587 = DIRECTION ( 'NONE',  ( -2.257144641399999941E-12, 0.000000000000000000, -1.000000000000000000 ) ) ;
#10588 = ORIENTED_EDGE ( 'NONE', *, *, #14141, .F. ) ;
#10589 = AXIS2_PLACEMENT_3D ( 'NONE', #9751, #15257, #6207 ) ;
#10590 = DIRECTION ( 'NONE',  ( 0.000000000000000000, 0.000000000000000000, 1.000000000000000000 ) ) ;
#10591 = EDGE_CURVE ( 'NONE', #6863, #7005, #8486, .T. ) ;
#10592 = CARTESIAN_POINT ( 'NONE',  ( 23.50000000000000000, -20.50000000000000000, -137.0552959530000123 ) ) ;
#10593 = VECTOR ( 'NONE', #18533, 1000.000000000000114 ) ;
#10594 = CARTESIAN_POINT ( 'NONE',  ( -34.50000000000000000, 48.00000000000000000, -139.5552959529999839 ) ) ;
#10595 = CARTESIAN_POINT ( 'NONE',  ( 7.268891187599542114, 37.85696889435310197, -141.7067652898295478 ) ) ;
#10596 = EDGE_LOOP ( 'NONE', ( #10777, #5885, #12308, #18566 ) ) ;
#10597 = DIRECTION ( 'NONE',  ( -1.000000000000000000, 0.000000000000000000, 2.273736754430000208E-12 ) ) ;
#10598 = EDGE_CURVE ( 'NONE', #4637, #6536, #8361, .T. ) ;
#10599 = CARTESIAN_POINT ( 'NONE',  ( -18.70471434392063514, 36.09242347422292596, -148.6518277728152100 ) ) ;
#10600 = DIRECTION ( 'NONE',  ( 2.257144641397284947E-12, -2.714760815920564689E-24, 1.000000000000000000 ) ) ;
#10601 = DIRECTION ( 'NONE',  ( -2.257242012349999735E-12, 0.000000000000000000, 1.000000000000000000 ) ) ;
#10602 = VERTEX_POINT ( 'NONE', #17300 ) ;
#10603 = CARTESIAN_POINT ( 'NONE',  ( -32.50000000000000000, 21.50000000000000000, -151.0552959529999839 ) ) ;
#10604 = AXIS2_PLACEMENT_3D ( 'NONE', #13943, #12500, #12269 ) ;
#10605 = CIRCLE ( 'NONE', #11742, 0.7500000000000006661 ) ;
#10606 = ORIENTED_EDGE ( 'NONE', *, *, #679, .T. ) ;
#10607 = FACE_OUTER_BOUND ( 'NONE', #795, .T. ) ;
#10608 = DIRECTION ( 'NONE',  ( 2.259525899719999991E-12, 0.000000000000000000, 1.000000000000000000 ) ) ;
#10609 = DIRECTION ( 'NONE',  ( -0.9874789572432817186, 0.1577507813030449846, 0.000000000000000000 ) ) ;
#10610 = AXIS2_PLACEMENT_3D ( 'NONE', #22808, #12080, #8149 ) ;
#10611 = EDGE_CURVE ( 'NONE', #18787, #1242, #7962, .T. ) ;
#10612 = VERTEX_POINT ( 'NONE', #783 ) ;
#10613 = VECTOR ( 'NONE', #17976, 1000.000000000000000 ) ;
#10614 = CARTESIAN_POINT ( 'NONE',  ( -4.584402860569999127, 37.05223431090000474, -140.2914745300000163 ) ) ;
#10615 = PLANE ( 'NONE',  #1154 ) ;
#10616 = VERTEX_POINT ( 'NONE', #15399 ) ;
#10617 = LINE ( 'NONE', #1620, #4964 ) ;
#10618 = FACE_BOUND ( 'NONE', #7108, .T. ) ;
#10619 = CARTESIAN_POINT ( 'NONE',  ( -14.80142434076114810, -44.50006722990159602, -150.0552959529999839 ) ) ;
#10620 = CARTESIAN_POINT ( 'NONE',  ( -9.394779979509999990, -17.86685386420000299, -143.5552959529999839 ) ) ;
#10621 = ADVANCED_FACE ( 'NONE', ( #1142 ), #10024, .F. ) ;
#10622 = CARTESIAN_POINT ( 'NONE',  ( -6.683153925719999222, -50.50000000000000000, -136.0552959530000123 ) ) ;
#10623 = DIRECTION ( 'NONE',  ( 0.7071067811865481278, -0.7071067811865469066, 1.776356839400246426E-12 ) ) ;
#10624 = PRODUCT_CONTEXT ( 'NONE', #16784, 'mechanical' ) ;
#10625 = LINE ( 'NONE', #7190, #646 ) ;
#10626 = EDGE_CURVE ( 'NONE', #15749, #22553, #12913, .T. ) ;
#10627 = VECTOR ( 'NONE', #22548, 1000.000000000000000 ) ;
#10628 = DIRECTION ( 'NONE',  ( -0.8020331419910812221, -0.5972795318340601289, 3.537910705138833522E-12 ) ) ;
#10629 = AXIS2_PLACEMENT_3D ( 'NONE', #14091, #21714, #19804 ) ;
#10630 = CARTESIAN_POINT ( 'NONE',  ( -13.92432874550000044, 37.01165864720000087, -139.5650670249999905 ) ) ;
#10631 = VECTOR ( 'NONE', #13631, 1000.000000000000000 ) ;
#10632 = ORIENTED_EDGE ( 'NONE', *, *, #5745, .F. ) ;
#10633 = UNCERTAINTY_MEASURE_WITH_UNIT (LENGTH_MEASURE( 1.000000000000000082E-05 ), #16607, 'distance_accuracy_value', 'NONE');
#10634 = VERTEX_POINT ( 'NONE', #13965 ) ;
#10635 = ORIENTED_EDGE ( 'NONE', *, *, #13452, .F. ) ;
#10636 = CARTESIAN_POINT ( 'NONE',  ( -16.16113997806470692, 37.07629171513308819, -147.8146678479332365 ) ) ;
#10637 = CARTESIAN_POINT ( 'NONE',  ( -28.00933461728345009, 33.78802393297787177, -142.0848207868532711 ) ) ;
#10638 = EDGE_LOOP ( 'NONE', ( #804, #5812, #2260, #12074 ) ) ;
#10639 = CARTESIAN_POINT ( 'NONE',  ( 18.95053822279999878, 50.00000000000000000, -150.5552959529999839 ) ) ;
#10640 = EDGE_LOOP ( 'NONE', ( #1824, #17509, #8392, #12598 ) ) ;
#10641 = CARTESIAN_POINT ( 'NONE',  ( 24.90191174488025538, 38.33948587668919572, -136.0552959530562021 ) ) ;
#10642 = CARTESIAN_POINT ( 'NONE',  ( -19.59255166816691940, 37.05126161860788159, -140.3061871180788103 ) ) ;
#10643 = CARTESIAN_POINT ( 'NONE',  ( -12.08222824379999949, 38.77433534089999512, -148.2726881729999775 ) ) ;
#10644 = DIRECTION ( 'NONE',  ( 0.000000000000000000, 1.000000000000000000, 0.000000000000000000 ) ) ;
#10645 = AXIS2_PLACEMENT_3D ( 'NONE', #13925, #4884, #12131 ) ;
#10646 = ORIENTED_EDGE ( 'NONE', *, *, #881, .T. ) ;
#10647 = VECTOR ( 'NONE', #9591, 1000.000000000000000 ) ;
#10648 = CYLINDRICAL_SURFACE ( 'NONE', #14083, 5.000000000000000888 ) ;
#10649 = EDGE_CURVE ( 'NONE', #22981, #12791, #9908, .T. ) ;
#10650 = ADVANCED_BREP_SHAPE_REPRESENTATION ( '', ( #11815, #5025 ), #21773 ) ;
#10651 = VERTEX_POINT ( 'NONE', #6476 ) ;
#10652 = CARTESIAN_POINT ( 'NONE',  ( 9.731108812837232946, 36.14303110608750558, -141.7067652896560617 ) ) ;
#10653 = PLANE ( 'NONE',  #12882 ) ;
#10654 = FACE_OUTER_BOUND ( 'NONE', #12418, .T. ) ;
#10655 = EDGE_CURVE ( 'NONE', #21497, #2284, #1548, .T. ) ;
#10656 = EDGE_LOOP ( 'NONE', ( #1890, #121, #10443, #17154, #18123, #7713 ) ) ;
#10657 = CARTESIAN_POINT ( 'NONE',  ( -32.50000000000000000, -43.00000000050000182, -137.0552959530000123 ) ) ;
#10658 = ORIENTED_EDGE ( 'NONE', *, *, #17582, .T. ) ;
#10659 = AXIS2_PLACEMENT_3D ( 'NONE', #13528, #938, #19130 ) ;
#10660 = PLANE ( 'NONE',  #4787 ) ;
#10661 = AXIS2_PLACEMENT_3D ( 'NONE', #991, #880, #2889 ) ;
#10662 = ORIENTED_EDGE ( 'NONE', *, *, #23478, .T. ) ;
#10663 = CARTESIAN_POINT ( 'NONE',  ( -12.28014746100000032, 36.97113097969999984, -148.4919582129999753 ) ) ;
#10664 = EDGE_LOOP ( 'NONE', ( #2954, #3667, #21768, #10584 ) ) ;
#10665 = CARTESIAN_POINT ( 'NONE',  ( -15.57415625657761282, 39.15353770086346685, -146.9238453625318925 ) ) ;
#10666 = ADVANCED_FACE ( 'NONE', ( #12054 ), #13487, .T. ) ;
#10667 = CARTESIAN_POINT ( 'NONE',  ( -3.500000000000000000, 42.50000000000000000, -150.0552959529999839 ) ) ;
#10668 = VERTEX_POINT ( 'NONE', #4574 ) ;
#10669 = ORIENTED_EDGE ( 'NONE', *, *, #13273, .T. ) ;
#10670 = CARTESIAN_POINT ( 'NONE',  ( -26.16983372419520038, 40.98399646752800152, -141.7700373851359927 ) ) ;
#10671 = CARTESIAN_POINT ( 'NONE',  ( 13.13369214859999978, 51.50000000000000000, -136.0552959530000123 ) ) ;
#10672 = ORIENTED_EDGE ( 'NONE', *, *, #10489, .F. ) ;
#10673 = DIRECTION ( 'NONE',  ( 1.211690350419999855E-27, 2.765629237170000203E-27, -1.000000000000000000 ) ) ;
#10674 = LINE ( 'NONE', #1671, #3051 ) ;
#10675 = ADVANCED_FACE ( 'NONE', ( #6704 ), #11373, .F. ) ;
#10676 = CARTESIAN_POINT ( 'NONE',  ( -30.02199999990000023, 40.89711431700000333, -146.3052959529999839 ) ) ;
#10677 = EDGE_LOOP ( 'NONE', ( #4175, #10016, #9217, #14594 ) ) ;
#10678 = EDGE_CURVE ( 'NONE', #22346, #19107, #5701, .T. ) ;
#10679 = CARTESIAN_POINT ( 'NONE',  ( -16.36784392970000113, 33.86562477380000047, -142.0582287350000001 ) ) ;
#10680 = CIRCLE ( 'NONE', #5386, 0.7500000000000006661 ) ;
#10681 = EDGE_CURVE ( 'NONE', #23345, #10651, #19324, .T. ) ;
#10682 = EDGE_CURVE ( 'NONE', #3418, #2622, #2560, .T. ) ;
#10683 = EDGE_LOOP ( 'NONE', ( #12922, #10317, #5690, #18998 ) ) ;
#10684 = PLANE ( 'NONE',  #21544 ) ;
#10685 = CARTESIAN_POINT ( 'NONE',  ( -11.65594158659679458, 36.92432879710134586, -140.1042033534126290 ) ) ;
#10686 =( REPRESENTATION_RELATIONSHIP ('NONE','NONE', #7672, #6919 ) REPRESENTATION_RELATIONSHIP_WITH_TRANSFORMATION ( #1975 )SHAPE_REPRESENTATION_RELATIONSHIP( ) );
#10687 = CARTESIAN_POINT ( 'NONE',  ( -14.31404048469557999, 38.45176613018656298, -140.7319883511174226 ) ) ;
#10688 = CARTESIAN_POINT ( 'NONE',  ( 10.68320006080000084, -20.50000000000000000, -148.5552959529999839 ) ) ;
#10689 = EDGE_LOOP ( 'NONE', ( #9240, #9536, #2463, #19821, #11642 ) ) ;
#10690 = CARTESIAN_POINT ( 'NONE',  ( -21.35824191589999899, -3.250000000000000000, -144.8157682190000060 ) ) ;
#10691 = CARTESIAN_POINT ( 'NONE',  ( 8.633772787779999902, -29.00605602609999778, -147.0552959529999839 ) ) ;
#10692 = DIRECTION ( 'NONE',  ( 0.000000000000000000, 0.000000000000000000, 1.000000000000000000 ) ) ;
#10693 = DIRECTION ( 'NONE',  ( 4.518783361002970486E-12, 0.000000000000000000, 1.000000000000000000 ) ) ;
#10694 = CARTESIAN_POINT ( 'NONE',  ( 19.13369214859999801, -50.50000000000000000, -136.5552959530000123 ) ) ;
#10695 = CARTESIAN_POINT ( 'NONE',  ( -37.07045745269999770, 37.00000000000000000, -139.0687076600000012 ) ) ;
#10696 = VECTOR ( 'NONE', #8879, 1000.000000000000227 ) ;
#10697 = VERTEX_POINT ( 'NONE', #3038 ) ;
#10698 = AXIS2_PLACEMENT_3D ( 'NONE', #21115, #8483, #13962 ) ;
#10699 = CIRCLE ( 'NONE', #19845, 7.499999999999999112 ) ;
#10700 = DIRECTION ( 'NONE',  ( 1.526468026909999897E-13, 8.159623473500000156E-13, 1.000000000000000000 ) ) ;
#10701 = CARTESIAN_POINT ( 'NONE',  ( 31.50000000000000000, 36.50000000000000000, -136.0552959530000123 ) ) ;
#10702 = CARTESIAN_POINT ( 'NONE',  ( 5.285243653077851711, -6.421918030004944100, -150.0552959529999839 ) ) ;
#10703 = CARTESIAN_POINT ( 'NONE',  ( -5.169538687456003423, 39.83360900324895937, -140.1488912727290881 ) ) ;
#10704 = DIRECTION ( 'NONE',  ( 0.7071067811865469066, 0.7071067811865481278, -1.591319668629387474E-12 ) ) ;
#10705 = ORIENTED_EDGE ( 'NONE', *, *, #18257, .T. ) ;
#10706 = ADVANCED_FACE ( 'NONE', ( #10275 ), #11813, .F. ) ;
#10707 = CARTESIAN_POINT ( 'NONE',  ( -9.434278515689999978, -18.41834002140000237, -147.5552959529999839 ) ) ;
#10708 = EDGE_CURVE ( 'NONE', #3831, #5244, #22547, .T. ) ;
#10709 = FACE_BOUND ( 'NONE', #8199, .T. ) ;
#10710 = EDGE_LOOP ( 'NONE', ( #8814, #9483, #16853, #8296 ) ) ;
#10711 = MECHANICAL_DESIGN_GEOMETRIC_PRESENTATION_REPRESENTATION (  '', ( #19841 ), #8444 ) ;
#10712 = DIRECTION ( 'NONE',  ( 7.105427352510001232E-15, -1.000000000000000000, -1.603797727360000188E-26 ) ) ;
#10713 = EDGE_LOOP ( 'NONE', ( #6845, #11178, #7217, #11466, #14958 ) ) ;
#10714 = CIRCLE ( 'NONE', #97, 6.000000000000001776 ) ;
#10715 = CARTESIAN_POINT ( 'NONE',  ( -23.96729089107739696, 37.81249143161688409, -148.2640374884782091 ) ) ;
#10716 = CARTESIAN_POINT ( 'NONE',  ( -29.32937220831407643, 40.41939957101111958, -140.7656299762568040 ) ) ;
#10717 = CARTESIAN_POINT ( 'NONE',  ( 22.27731556082403941, -15.33058227694559683, -144.5552959530006945 ) ) ;
#10718 = CARTESIAN_POINT ( 'NONE',  ( 7.774829774480637390, 38.31328358559468228, -141.9279471761695675 ) ) ;
#10719 = ORIENTED_EDGE ( 'NONE', *, *, #9125, .T. ) ;
#10720 = CARTESIAN_POINT ( 'NONE',  ( -9.944031889410000602, 32.62729151690000151, -143.2983400859999961 ) ) ;
#10721 = CARTESIAN_POINT ( 'NONE',  ( -18.99012760142337441, 32.85953695965795873, -141.8126290792370696 ) ) ;
#10722 = CARTESIAN_POINT ( 'NONE',  ( -9.174907861666381947, 40.57495297524849320, -144.3653690793416615 ) ) ;
#10723 = CARTESIAN_POINT ( 'NONE',  ( 3.906463970600278834, -34.75246044238718923, -136.0552959530088231 ) ) ;
#10724 = VERTEX_POINT ( 'NONE', #10735 ) ;
#10725 = CARTESIAN_POINT ( 'NONE',  ( 2.508811538190000245, -14.35090895149999923, -145.0552959529999839 ) ) ;
#10726 =( NAMED_UNIT ( * ) SI_UNIT ( $, .STERADIAN. ) SOLID_ANGLE_UNIT ( ) );
#10727 = ORIENTED_EDGE ( 'NONE', *, *, #5242, .F. ) ;
#10728 = CARTESIAN_POINT ( 'NONE',  ( -10.49999999989999822, 37.00000000000000000, -144.0552959529999839 ) ) ;
#10729 = CARTESIAN_POINT ( 'NONE',  ( -6.288682381900000173, 41.28368337119999865, -144.4167712529999790 ) ) ;
#10730 =( GEOMETRIC_REPRESENTATION_CONTEXT ( 3 ) GLOBAL_UNCERTAINTY_ASSIGNED_CONTEXT ( ( #1384 ) ) GLOBAL_UNIT_ASSIGNED_CONTEXT ( ( #11513, #3491, #20694 ) ) REPRESENTATION_CONTEXT ( 'NONE', 'WORKASPACE' ) );
#10731 = DIRECTION ( 'NONE',  ( -0.7633862853691524286, -0.6459422414661292189, -2.187565684150435883E-17 ) ) ;
#10732 = CIRCLE ( 'NONE', #7694, 1.499999999999999556 ) ;
#10733 = ORIENTED_EDGE ( 'NONE', *, *, #18564, .F. ) ;
#10734 = EDGE_CURVE ( 'NONE', #22797, #21113, #12292, .T. ) ;
#10735 = CARTESIAN_POINT ( 'NONE',  ( -12.50000000000000000, 42.50000000000000000, -151.0552959529999839 ) ) ;
#10736 = DIRECTION ( 'NONE',  ( -0.7432941462487078210, 0.000000000000000000, -0.6689647316207368855 ) ) ;
#10737 = ORIENTED_EDGE ( 'NONE', *, *, #3717, .T. ) ;
#10738 = DIRECTION ( 'NONE',  ( 5.094701932209999624E-24, 1.000000000000000000, -1.149947916579999802E-35 ) ) ;
#10739 = CARTESIAN_POINT ( 'NONE',  ( 18.98537695655051394, 19.88080765318867194, -150.0552959530000123 ) ) ;
#10740 = DIRECTION ( 'NONE',  ( 1.000000000000000000, -1.190078432789999897E-50, -2.257144641399999941E-12 ) ) ;
#10741 = DIRECTION ( 'NONE',  ( -1.000000000000000000, 0.000000000000000000, 0.000000000000000000 ) ) ;
#10742 = CYLINDRICAL_SURFACE ( 'NONE', #3275, 3.000000000000000000 ) ;
#10743 = LINE ( 'NONE', #12658, #18137 ) ;
#10744 = ITEM_DEFINED_TRANSFORMATION ( 'NONE', 'NONE', #16470,  #5025 ) ;
#10745 = DIRECTION ( 'NONE',  ( -1.000000000000000000, -3.994014902950000436E-29, 0.000000000000000000 ) ) ;
#10746 = AXIS2_PLACEMENT_3D ( 'NONE', #23305, #6877, #3312 ) ;
#10747 = CARTESIAN_POINT ( 'NONE',  ( 12.82492181439999968, -17.92284828160000032, -145.5552959529999839 ) ) ;
#10748 = CARTESIAN_POINT ( 'NONE',  ( 18.95053822279999878, -50.00000000000000000, -149.5552959529999839 ) ) ;
#10749 = ORIENTED_EDGE ( 'NONE', *, *, #11680, .F. ) ;
#10750 = ORIENTED_EDGE ( 'NONE', *, *, #303, .F. ) ;
#10751 = VERTEX_POINT ( 'NONE', #15864 ) ;
#10752 = FACE_BOUND ( 'NONE', #14240, .T. ) ;
#10753 = DIRECTION ( 'NONE',  ( 0.000000000000000000, -1.000000000000000000, -2.765629237170000203E-27 ) ) ;
#10754 = DIRECTION ( 'NONE',  ( 1.000000000000000000, 0.000000000000000000, -4.429789868254373788E-12 ) ) ;
#10755 = CARTESIAN_POINT ( 'NONE',  ( 12.46241645107507168, 25.07592078381926015, -136.0552959530281214 ) ) ;
#10756 = VERTEX_POINT ( 'NONE', #8711 ) ;
#10757 = ADVANCED_FACE ( 'NONE', ( #1841 ), #21828, .T. ) ;
#10758 = CARTESIAN_POINT ( 'NONE',  ( -5.660609041639971473, 24.90181682660303508, -150.0552959529999839 ) ) ;
#10759 = DIRECTION ( 'NONE',  ( 1.000000000000000000, 0.000000000000000000, 2.516505522483685870E-12 ) ) ;
#10760 = CARTESIAN_POINT ( 'NONE',  ( -11.53909816450000037, 41.50279269539999660, -144.7127947380000137 ) ) ;
#10761 = ADVANCED_FACE ( 'NONE', ( #12647 ), #16229, .T. ) ;
#10762 = DIRECTION ( 'NONE',  ( 4.123791986225375161E-10, 0.000000000000000000, -1.000000000000000000 ) ) ;
#10763 = VERTEX_POINT ( 'NONE', #23368 ) ;
#10764 = CARTESIAN_POINT ( 'NONE',  ( 8.463109132734597750, 13.19520492498762998, -136.0552959530044461 ) ) ;
#10765 = AXIS2_PLACEMENT_3D ( 'NONE', #7088, #1750, #23508 ) ;
#10766 = ORIENTED_EDGE ( 'NONE', *, *, #19490, .F. ) ;
#10767 = LINE ( 'NONE', #7097, #6032 ) ;
#10768 = LINE ( 'NONE', #12090, #17061 ) ;
#10769 = CYLINDRICAL_SURFACE ( 'NONE', #20515, 1.000000000000001332 ) ;
#10770 = ORIENTED_EDGE ( 'NONE', *, *, #11550, .F. ) ;
#10771 = FACE_OUTER_BOUND ( 'NONE', #10287, .T. ) ;
#10772 = VERTEX_POINT ( 'NONE', #12177 ) ;
#10773 = PLANE ( 'NONE',  #6001 ) ;
#10774 = DIRECTION ( 'NONE',  ( -1.000000000000000000, 0.000000000000000000, 2.256683728769999802E-12 ) ) ;
#10775 = ORIENTED_EDGE ( 'NONE', *, *, #15787, .T. ) ;
#10776 = FACE_OUTER_BOUND ( 'NONE', #8349, .T. ) ;
#10777 = ORIENTED_EDGE ( 'NONE', *, *, #17549, .T. ) ;
#10778 = VECTOR ( 'NONE', #18936, 1000.000000000000000 ) ;
#10779 = CARTESIAN_POINT ( 'NONE',  ( -21.93648690846499605, 37.04947573026642971, -148.4875734863409775 ) ) ;
#10780 = CARTESIAN_POINT ( 'NONE',  ( -4.726769794318020246, 42.89852487308611018, -150.0552959529999839 ) ) ;
#10781 = ORIENTED_EDGE ( 'NONE', *, *, #5376, .F. ) ;
#10782 = DIRECTION ( 'NONE',  ( 0.000000000000000000, 0.000000000000000000, 1.000000000000000000 ) ) ;
#10783 = VERTEX_POINT ( 'NONE', #18129 ) ;
#10784 = CARTESIAN_POINT ( 'NONE',  ( -26.81858241934068943, 38.72415308318589666, -139.9577798820823489 ) ) ;
#10785 = LINE ( 'NONE', #3202, #9572 ) ;
#10786 = ORIENTED_EDGE ( 'NONE', *, *, #10334, .F. ) ;
#10787 = EDGE_CURVE ( 'NONE', #19696, #11665, #20917, .T. ) ;
#10788 = DIRECTION ( 'NONE',  ( 0.000000000000000000, 0.000000000000000000, -1.000000000000000000 ) ) ;
#10789 = CARTESIAN_POINT ( 'NONE',  ( -10.33840623949446424, 36.25694129130458521, -139.9440796118479398 ) ) ;
#10790 = CARTESIAN_POINT ( 'NONE',  ( -32.50000000000000000, -36.00000000000000000, -149.5552959529999839 ) ) ;
#10791 = ORIENTED_EDGE ( 'NONE', *, *, #16635, .F. ) ;
#10792 = CARTESIAN_POINT ( 'NONE',  ( -15.76532943049999780, 34.76918918230000344, -146.9254579969999952 ) ) ;
#10793 = ADVANCED_FACE ( 'NONE', ( #19452 ), #14443, .T. ) ;
#10794 = ORIENTED_EDGE ( 'NONE', *, *, #14548, .T. ) ;
#10795 = FACE_OUTER_BOUND ( 'NONE', #17164, .T. ) ;
#10796 = LINE ( 'NONE', #18200, #16541 ) ;
#10797 = CARTESIAN_POINT ( 'NONE',  ( -15.46613156839596037, 36.99333119720399310, -147.5584717933712113 ) ) ;
#10798 = DIRECTION ( 'NONE',  ( 2.257171095940000041E-12, 1.003664318210000046E-28, 1.000000000000000000 ) ) ;
#10799 = ORIENTED_EDGE ( 'NONE', *, *, #6629, .F. ) ;
#10800 =( NAMED_UNIT ( * ) PLANE_ANGLE_UNIT ( ) SI_UNIT ( $, .RADIAN. ) );
#10801 = DIRECTION ( 'NONE',  ( 0.000000000000000000, 2.257144641399999941E-12, -1.000000000000000000 ) ) ;
#10802 = ADVANCED_FACE ( 'NONE', ( #7300 ), #21359, .T. ) ;
#10803 = B_SPLINE_CURVE_WITH_KNOTS ( 'NONE', 3,
 ( #3381, #17307, #10280, #17552, #1269, #14570, #59, #19809, #11093, #10619, #10977, #16355, #3736, #21946, #7068, #5281, #12654, #22060 ),
 .UNSPECIFIED., .F., .F.,
 ( 4, 2, 2, 2, 2, 2, 2, 2, 4 ),
 ( 0.000000000000000000, 0.1250000000000000000, 0.2500000000000000000, 0.3750000000000000000, 0.5000000000000000000, 0.6250000000000000000, 0.7500000000000000000, 0.8750000000000000000, 1.000000000000000000 ),
 .UNSPECIFIED. ) ;
#10804 = DIRECTION ( 'NONE',  ( 1.000000000000000000, 0.000000000000000000, -1.498801083243961330E-13 ) ) ;
#10805 = CARTESIAN_POINT ( 'NONE',  ( -33.50000000000000000, 46.00000000000000000, -146.5552959529999839 ) ) ;
#10806 = DIRECTION ( 'NONE',  ( 0.000000000000000000, 1.000000000000000000, 0.000000000000000000 ) ) ;
#10807 = DIRECTION ( 'NONE',  ( 2.839308199620000013E-14, 3.568879590630000244E-13, 1.000000000000000000 ) ) ;
#10808 = ORIENTED_EDGE ( 'NONE', *, *, #15642, .T. ) ;
#10809 = CARTESIAN_POINT ( 'NONE',  ( 19.77963439019999825, -51.26338628519999929, -149.5552959529999839 ) ) ;
#10810 = ADVANCED_FACE ( 'NONE', ( #19565 ), #15990, .F. ) ;
#10811 = DIRECTION ( 'NONE',  ( -1.000000000000000000, 0.000000000000000000, 0.000000000000000000 ) ) ;
#10812 = PLANE ( 'NONE',  #1884 ) ;
#10813 = ADVANCED_FACE ( 'NONE', ( #23251 ), #14319, .T. ) ;
#10814 = AXIS2_PLACEMENT_3D ( 'NONE', #20829, #11417, #22262 ) ;
#10815 = CARTESIAN_POINT ( 'NONE',  ( -6.010199571182928580, 41.30249798234603986, -146.4953287552840777 ) ) ;
#10816 = CARTESIAN_POINT ( 'NONE',  ( 1.829659965300000080, -16.02499107890000118, -144.0552959529999839 ) ) ;
#10817 = ORIENTED_EDGE ( 'NONE', *, *, #15497, .F. ) ;
#10818 = CARTESIAN_POINT ( 'NONE',  ( 10.68320006080000084, -21.50000000000000000, -148.5552959529999839 ) ) ;
#10819 = FACE_BOUND ( 'NONE', #8807, .T. ) ;
#10820 = EDGE_LOOP ( 'NONE', ( #9163, #20116 ) ) ;
#10821 = EDGE_CURVE ( 'NONE', #1892, #22553, #3497, .T. ) ;
#10822 = CARTESIAN_POINT ( 'NONE',  ( -25.10891061333512653, 37.07005729393354443, -148.1636427046708491 ) ) ;
#10823 = ORIENTED_EDGE ( 'NONE', *, *, #17238, .T. ) ;
#10824 = EDGE_CURVE ( 'NONE', #2894, #14227, #22813, .T. ) ;
#10825 = DIRECTION ( 'NONE',  ( 5.094701932209999624E-24, 1.000000000000000000, 0.000000000000000000 ) ) ;
#10826 = CARTESIAN_POINT ( 'NONE',  ( -29.55850978546380148, 41.47329217817320313, -142.4456950392549857 ) ) ;
#10827 = CARTESIAN_POINT ( 'NONE',  ( -22.23138069770000058, 34.62558912630000663, -140.6296127990000002 ) ) ;
#10828 = CARTESIAN_POINT ( 'NONE',  ( 7.009192481380154049, 36.80638614241070883, -141.5610522423419866 ) ) ;
#10829 = CIRCLE ( 'NONE', #18076, 9.999999999999998224 ) ;
#10830 = ORIENTED_EDGE ( 'NONE', *, *, #3769, .T. ) ;
#10831 = CARTESIAN_POINT ( 'NONE',  ( -10.50749457979810586, 32.24767484617476754, -143.3007931252695073 ) ) ;
#10832 = VECTOR ( 'NONE', #8842, 1000.000000000000000 ) ;
#10833 = CARTESIAN_POINT ( 'NONE',  ( -19.14968637899999848, 34.49201595030000078, -147.7870032629999741 ) ) ;
#10834 = ADVANCED_FACE ( 'NONE', ( #16113 ), #21943, .F. ) ;
#10835 = CARTESIAN_POINT ( 'NONE',  ( -8.932337917339909339, 37.68960189247532355, -147.6085193066813304 ) ) ;
#10836 = CARTESIAN_POINT ( 'NONE',  ( -34.50000000000000000, -65.45885107719999496, -145.8104610769999852 ) ) ;
#10837 = VERTEX_POINT ( 'NONE', #9294 ) ;
#10838 = EDGE_CURVE ( 'NONE', #6870, #4401, #16567, .T. ) ;
#10839 = CARTESIAN_POINT ( 'NONE',  ( 19.71940181160250560, 25.42378041200771221, -136.0552959530445207 ) ) ;
#10840 = PRESENTATION_STYLE_ASSIGNMENT (( #16220 ) ) ;
#10841 = ADVANCED_FACE ( 'NONE', ( #18938 ), #2772, .T. ) ;
#10842 = ORIENTED_EDGE ( 'NONE', *, *, #15785, .T. ) ;
#10843 = PLANE ( 'NONE',  #2375 ) ;
#10844 = DIRECTION ( 'NONE',  ( 2.507771768019999718E-12, 1.592654864209999947E-17, -1.000000000000000000 ) ) ;
#10845 = FACE_OUTER_BOUND ( 'NONE', #19303, .T. ) ;
#10846 = ORIENTED_EDGE ( 'NONE', *, *, #7602, .F. ) ;
#10847 = CARTESIAN_POINT ( 'NONE',  ( -5.746192911800908298, 37.73100506242058572, -140.1565350977006119 ) ) ;
#10848 = CARTESIAN_POINT ( 'NONE',  ( -4.499999999959999109, -2.273736754430000208E-12, -136.0552959530000123 ) ) ;
#10849 = AXIS2_PLACEMENT_3D ( 'NONE', #8525, #21166, #12331 ) ;
#10850 = CIRCLE ( 'NONE', #13909, 35.00000000000000000 ) ;
#10851 = VERTEX_POINT ( 'NONE', #17275 ) ;
#10852 = LINE ( 'NONE', #19679, #1175 ) ;
#10853 = B_SPLINE_CURVE_WITH_KNOTS ( 'NONE', 5,
 ( #13212, #20487, #13562, #20834, #18706, #2415, #16906, #22386, #4303, #11533, #22729, #23207 ),
 .UNSPECIFIED., .F., .F.,
 ( 6, 3, 3, 6 ),
 ( 0.000000000000000000, 4.371092480729999785, 8.745625541600000830, 13.12578902609999965 ),
 .UNSPECIFIED. ) ;
#10854 = DIRECTION ( 'NONE',  ( 1.000000000000000000, 2.602084704489999637E-17, -1.701177084830000066E-20 ) ) ;
#10855 = DIRECTION ( 'NONE',  ( 2.257157423930000049E-12, 0.000000000000000000, 1.000000000000000000 ) ) ;
#10856 = CARTESIAN_POINT ( 'NONE',  ( 19.68320006079999729, -20.50000000000000000, -150.0552959529999839 ) ) ;
#10857 = DIRECTION ( 'NONE',  ( -0.000000000000000000, 1.000000000000000000, 0.000000000000000000 ) ) ;
#10858 = CARTESIAN_POINT ( 'NONE',  ( -9.282104535849999394, -16.71402168319999859, -144.5552959529999839 ) ) ;
#10859 = ITEM_DEFINED_TRANSFORMATION ( 'NONE', 'NONE', #17992,  #5025 ) ;
#10860 = DIRECTION ( 'NONE',  ( 0.000000000000000000, -1.000000000000000000, 0.000000000000000000 ) ) ;
#10861 = CARTESIAN_POINT ( 'NONE',  ( 4.750000000000000000, -47.00000000000000000, -150.0552959529999839 ) ) ;
#10862 =( BOUNDED_SURFACE ( )  B_SPLINE_SURFACE ( 5, 5, ( 
 ( #7868, #13230, #2434, #4080, #758, #9886 ),
 ( #14915, #4322, #18725, #2660, #9414, #4207 ),
 ( #11552, #17160, #4431, #882, #2539, #15143 ),
 ( #11201, #22526, #18828, #13115, #6102, #9651 ),
 ( #16923, #635, #22406, #7642, #20508, #13354 ),
 ( #15379, #16813, #20627, #16691, #13467, #3969 ),
 ( #9762, #17039, #6329, #7988, #22286, #18476 ),
 ( #6219, #406, #11667, #11441, #20388, #11318 ),
 ( #18599, #9541, #525, #7757, #15021, #2169 ),
 ( #22150, #7734, #21924, #4181, #16900, #18569 ),
 ( #6078, #9390, #20256, #20599, #5951, #13092 ),
 ( #22377, #5836, #20363, #5605, #16444, #4058 ) ),
 .UNSPECIFIED., .F., .F., .F. ) 
 B_SPLINE_SURFACE_WITH_KNOTS ( ( 6, 3, 3, 6 ),
 ( 6, 6 ),
 ( 0.000000000000000000, 4.463483057499999518, 8.880954762089999122, 13.25426345570000031 ),
 ( 1.570796326503985041, 3.141592653590000062 ),
 .UNSPECIFIED. ) 
 GEOMETRIC_REPRESENTATION_ITEM ( )  RATIONAL_B_SPLINE_SURFACE ( (
 ( 0.2500000000000000000, 0.2499999999629470004, 0.2999999999444205034, 0.3999999999258939676, 0.5999999999258940342, 1.000000000000000000),
 ( 0.2500000000000000000, 0.2499999999629470004, 0.2999999999444205034, 0.3999999999258939676, 0.5999999999258940342, 1.000000000000000000),
 ( 0.2500000000000000000, 0.2499999999629470004, 0.2999999999444205034, 0.3999999999258939676, 0.5999999999258940342, 1.000000000000000000),
 ( 0.2500000000000000000, 0.2499999999629470004, 0.2999999999444205034, 0.3999999999258939676, 0.5999999999258940342, 1.000000000000000000),
 ( 0.2500000000000000000, 0.2499999999629470004, 0.2999999999444205034, 0.3999999999258939676, 0.5999999999258940342, 1.000000000000000000),
 ( 0.2500000000000000000, 0.2499999999629470004, 0.2999999999444205034, 0.3999999999258939676, 0.5999999999258940342, 1.000000000000000000),
 ( 0.2500000000000000000, 0.2499999999629470004, 0.2999999999444205034, 0.3999999999258939676, 0.5999999999258940342, 1.000000000000000000),
 ( 0.2500000000000000000, 0.2499999999629470004, 0.2999999999444205034, 0.3999999999258939676, 0.5999999999258940342, 1.000000000000000000),
 ( 0.2500000000000000000, 0.2499999999629470004, 0.2999999999444205034, 0.3999999999258939676, 0.5999999999258940342, 1.000000000000000000),
 ( 0.2500000000000000000, 0.2499999999629470004, 0.2999999999444205034, 0.3999999999258939676, 0.5999999999258940342, 1.000000000000000000),
 ( 0.2500000000000000000, 0.2499999999629470004, 0.2999999999444205034, 0.3999999999258939676, 0.5999999999258940342, 1.000000000000000000),
 ( 0.2500000000000000000, 0.2499999999629470004, 0.2999999999444205034, 0.3999999999258939676, 0.5999999999258940342, 1.000000000000000000) ) ) 
 REPRESENTATION_ITEM ( '' )  SURFACE ( )  );
#10863 = EDGE_CURVE ( 'NONE', #22307, #3022, #13828, .T. ) ;
#10864 = CARTESIAN_POINT ( 'NONE',  ( 31.50000000000000000, 20.96379895120000114, -136.0552959530000123 ) ) ;
#10865 = VERTEX_POINT ( 'NONE', #22875 ) ;
#10866 = EDGE_CURVE ( 'NONE', #10483, #2706, #4781, .T. ) ;
#10867 = CIRCLE ( 'NONE', #16584, 2.000000000000001776 ) ;
#10868 = UNCERTAINTY_MEASURE_WITH_UNIT (LENGTH_MEASURE( 1.000000000000000082E-05 ), #13599, 'distance_accuracy_value', 'NONE');
#10869 = EDGE_LOOP ( 'NONE', ( #444, #10120, #18030, #20468 ) ) ;
#10870 = DIRECTION ( 'NONE',  ( 1.000000000000000000, 0.000000000000000000, 0.000000000000000000 ) ) ;
#10871 = VERTEX_POINT ( 'NONE', #22631 ) ;
#10872 = CARTESIAN_POINT ( 'NONE',  ( 29.68320006080000084, -28.50000000000000000, -150.0552959529999839 ) ) ;
#10873 = CARTESIAN_POINT ( 'NONE',  ( -13.47473365134610290, 34.60989327097050250, -147.6241178362156745 ) ) ;
#10874 = ORIENTED_EDGE ( 'NONE', *, *, #7065, .F. ) ;
#10875 = CARTESIAN_POINT ( 'NONE',  ( 22.50000000000000000, 33.50000000000000000, -150.5552959529999839 ) ) ;
#10876 = ORIENTED_EDGE ( 'NONE', *, *, #7117, .F. ) ;
#10877 = FACE_OUTER_BOUND ( 'NONE', #15194, .T. ) ;
#10878 = CARTESIAN_POINT ( 'NONE',  ( -19.17479249162562027, 35.04308797501523287, -146.9876367767126908 ) ) ;
#10879 = CARTESIAN_POINT ( 'NONE',  ( -12.76385253892641991, 37.02886902030763849, -147.6186336935359975 ) ) ;
#10880 = CARTESIAN_POINT ( 'NONE',  ( -25.85824191589999899, -13.50000000000000000, -146.3157682190000060 ) ) ;
#10881 = VERTEX_POINT ( 'NONE', #1105 ) ;
#10882 = FACE_BOUND ( 'NONE', #2961, .T. ) ;
#10883 = ORIENTED_EDGE ( 'NONE', *, *, #10388, .F. ) ;
#10884 = DIRECTION ( 'NONE',  ( -0.1435602414469281940, -0.9896415801065048257, 3.836930773098079160E-13 ) ) ;
#10885 = VECTOR ( 'NONE', #23493, 1000.000000000000000 ) ;
#10886 = LINE ( 'NONE', #18166, #228 ) ;
#10887 = CARTESIAN_POINT ( 'NONE',  ( 16.25412235410000150, -22.59491385829999999, -146.5552959529999839 ) ) ;
#10888 = ORIENTED_EDGE ( 'NONE', *, *, #21483, .T. ) ;
#10889 = ADVANCED_FACE ( 'NONE', ( #19296 ), #13733, .F. ) ;
#10890 = ADVANCED_FACE ( 'NONE', ( #22988 ), #3914, .F. ) ;
#10891 = LINE ( 'NONE', #22207, #12571 ) ;
#10892 = ORIENTED_EDGE ( 'NONE', *, *, #18244, .F. ) ;
#10893 = ADVANCED_FACE ( 'NONE', ( #13936 ), #21533, .T. ) ;
#10894 = DIRECTION ( 'NONE',  ( 0.000000000000000000, 1.000000000000000000, 0.000000000000000000 ) ) ;
#10896 = ORIENTED_EDGE ( 'NONE', *, *, #8377, .T. ) ;
#10895 = AXIS2_PLACEMENT_3D ( 'NONE', #17908, #6714, #13976 ) ;
#10897 = CARTESIAN_POINT ( 'NONE',  ( -26.87491139698960652, 40.50028737762694675, -144.3978882166674396 ) ) ;
#10898 = ORIENTED_EDGE ( 'NONE', *, *, #21483, .F. ) ;
#10899 = CARTESIAN_POINT ( 'NONE',  ( -15.47708384459999920, 37.95279615419999431, -148.5507537150000132 ) ) ;
#10900 = CIRCLE ( 'NONE', #288, 2.500000000000002220 ) ;
#10901 = DIRECTION ( 'NONE',  ( -0.7633862853691524286, -0.6459422414661292189, 2.734434900580546249E-18 ) ) ;
#10902 = VERTEX_POINT ( 'NONE', #21654 ) ;
#10903 = ORIENTED_EDGE ( 'NONE', *, *, #16925, .T. ) ;
#10904 = CARTESIAN_POINT ( 'NONE',  ( -27.29484193126405600, 40.93981164352350532, -143.5422035504862208 ) ) ;
#10905 = DIRECTION ( 'NONE',  ( -3.994014902950000436E-29, 1.000000000000000000, -4.148443855749999753E-27 ) ) ;
#10906 = ORIENTED_EDGE ( 'NONE', *, *, #21107, .T. ) ;
#10907 = CARTESIAN_POINT ( 'NONE',  ( 31.50000000010000178, 40.03620104870000063, -149.5552959529999839 ) ) ;
#10908 = CARTESIAN_POINT ( 'NONE',  ( -3.499999999969999998, 34.00000000000000000, -137.0552959530000123 ) ) ;
#10909 = CARTESIAN_POINT ( 'NONE',  ( 32.05742780199999942, -40.87448416760000214, -150.0552959529999839 ) ) ;
#10910 = ORIENTED_EDGE ( 'NONE', *, *, #7457, .T. ) ;
#10911 = LINE ( 'NONE', #9131, #1112 ) ;
#10912 = AXIS2_PLACEMENT_3D ( 'NONE', #19874, #4033, #23435 ) ;
#10913 = PLANE ( 'NONE',  #9065 ) ;
#10914 = ORIENTED_EDGE ( 'NONE', *, *, #8617, .F. ) ;
#10915 = DIRECTION ( 'NONE',  ( 0.000000000000000000, -1.000000000000000000, 0.000000000000000000 ) ) ;
#10916 = LINE ( 'NONE', #3325, #8542 ) ;
#10917 = EDGE_CURVE ( 'NONE', #14032, #4852, #14065, .T. ) ;
#10918 = CARTESIAN_POINT ( 'NONE',  ( -17.01025018545970013, 38.48180121062596015, -140.7067500820750183 ) ) ;
#10919 = CARTESIAN_POINT ( 'NONE',  ( -29.49311769368501857, 40.53847605628178741, -144.3259011655036375 ) ) ;
#10920 = VERTEX_POINT ( 'NONE', #19973 ) ;
#10921 = CARTESIAN_POINT ( 'NONE',  ( 0.5375835489975798742, 15.92407921618114663, -136.0552959530012345 ) ) ;
#10922 = EDGE_CURVE ( 'NONE', #6748, #20191, #10674, .T. ) ;
#10923 = CARTESIAN_POINT ( 'NONE',  ( 16.64676602990000021, -18.64223989710000140, -143.5552959529999839 ) ) ;
#10924 = PLANE ( 'NONE',  #14476 ) ;
#10925 = CARTESIAN_POINT ( 'NONE',  ( -2.499999999929999994, 34.00000000000000000, -138.0552959530000123 ) ) ;
#10926 = CARTESIAN_POINT ( 'NONE',  ( 4.999999999879999990, -2.250000000000000000, -135.4552959529999896 ) ) ;
#10927 = DIRECTION ( 'NONE',  ( 0.000000000000000000, -1.000000000000000000, 0.000000000000000000 ) ) ;
#10928 = ORIENTED_EDGE ( 'NONE', *, *, #12597, .T. ) ;
#10929 = DIRECTION ( 'NONE',  ( 1.000000000000000000, 0.000000000000000000, -1.527536832333223921E-13 ) ) ;
#10931 = CIRCLE ( 'NONE', #9397, 9.000000000000000000 ) ;
#10930 = PRODUCT_DEFINITION ( 'UNKNOWN', '', #22938, #16585 ) ;
#10932 = DIRECTION ( 'NONE',  ( 1.000000000000000000, 0.000000000000000000, -2.257144641399999941E-12 ) ) ;
#10933 = CARTESIAN_POINT ( 'NONE',  ( 19.04211518569999839, 51.50000000000000000, -149.5552959529999839 ) ) ;
#10934 = EDGE_CURVE ( 'NONE', #1717, #4754, #16345, .T. ) ;
#10935 = AXIS2_PLACEMENT_3D ( 'NONE', #16037, #17942, #5086 ) ;
#10936 = CARTESIAN_POINT ( 'NONE',  ( -6.064688046277384004, 37.92358258467430687, -148.6337691084673338 ) ) ;
#10937 = CARTESIAN_POINT ( 'NONE',  ( 1.133692148550000001, -51.50000000000000000, -137.0552959530000123 ) ) ;
#10938 = ORIENTED_EDGE ( 'NONE', *, *, #11697, .T. ) ;
#10939 = CARTESIAN_POINT ( 'NONE',  ( 16.25412235410000150, -22.59491385829999999, -145.5552959529999839 ) ) ;
#10940 = CARTESIAN_POINT ( 'NONE',  ( 4.750000000030000002, -35.98606797749999942, -136.0552959530000123 ) ) ;
#10941 = ORIENTED_EDGE ( 'NONE', *, *, #1084, .T. ) ;
#10942 = EDGE_CURVE ( 'NONE', #2120, #16131, #7121, .T. ) ;
#10943 = CARTESIAN_POINT ( 'NONE',  ( 10.93320006080000084, -15.50000000000000000, -138.5552959529999839 ) ) ;
#10944 = ORIENTED_EDGE ( 'NONE', *, *, #20315, .F. ) ;
#10945 = CARTESIAN_POINT ( 'NONE',  ( -24.06602356380263785, 36.94557182218072455, -148.2530914613568029 ) ) ;
#10946 = VECTOR ( 'NONE', #725, 1000.000000000000000 ) ;
#10947 = VECTOR ( 'NONE', #3912, 1000.000000000000000 ) ;
#10948 = CARTESIAN_POINT ( 'NONE',  ( -46.29070078859999882, 46.25000000000000000, -147.5552959529999839 ) ) ;
#10949 = VECTOR ( 'NONE', #20237, 1000.000000000000000 ) ;
#10950 = DIRECTION ( 'NONE',  ( 9.087266560786239640E-12, 0.000000000000000000, 1.000000000000000000 ) ) ;
#10951 = CARTESIAN_POINT ( 'NONE',  ( 7.848660272661017068, 35.64846932482826958, -141.9520366272613501 ) ) ;
#10952 = ORIENTED_EDGE ( 'NONE', *, *, #5041, .F. ) ;
#10953 = CARTESIAN_POINT ( 'NONE',  ( -11.08944297849076399, 33.05461395872589492, -141.6094732493307617 ) ) ;
#10954 = EDGE_CURVE ( 'NONE', #20932, #802, #12589, .T. ) ;
#10955 = CARTESIAN_POINT ( 'NONE',  ( -19.10658510145665900, 32.20893999946100195, -143.7553378037570155 ) ) ;
#10956 = DIRECTION ( 'NONE',  ( -0.9694775522152123681, 0.2451800884060535979, 8.905086759541945709E-12 ) ) ;
#10957 = CARTESIAN_POINT ( 'NONE',  ( 7.351088731987364788, -30.79529868152849303, -136.0552959530165822 ) ) ;
#10958 = AXIS2_PLACEMENT_3D ( 'NONE', #7123, #9129, #1672 ) ;
#10959 = CARTESIAN_POINT ( 'NONE',  ( -23.54789306461707810, 36.93722613941657329, -139.7713821669954370 ) ) ;
#10960 = EDGE_LOOP ( 'NONE', ( #9084, #8489, #13276, #16662 ) ) ;
#10961 = DIRECTION ( 'NONE',  ( 1.000000000000000000, 0.000000000000000000, -2.257453483404484831E-12 ) ) ;
#10962 = EDGE_CURVE ( 'NONE', #19736, #1038, #3675, .T. ) ;
#10963 = FACE_BOUND ( 'NONE', #2431, .T. ) ;
#10964 = CARTESIAN_POINT ( 'NONE',  ( 18.95053822279999878, 50.50000000000000000, -149.5552959529999839 ) ) ;
#10965 = CARTESIAN_POINT ( 'NONE',  ( -5.985376956567993290, 25.11919234682552116, -136.0552959529864552 ) ) ;
#10966 = AXIS2_PLACEMENT_3D ( 'NONE', #23487, #10854, #14095 ) ;
#10967 = ORIENTED_EDGE ( 'NONE', *, *, #22277, .F. ) ;
#10968 = CARTESIAN_POINT ( 'NONE',  ( -6.705189174517019346, 39.56570632389819764, -147.4373625594447788 ) ) ;
#10969 = VECTOR ( 'NONE', #20663, 1000.000000000000000 ) ;
#10970 = EDGE_LOOP ( 'NONE', ( #14883, #21545, #1868, #3367 ) ) ;
#10971 = FACE_OUTER_BOUND ( 'NONE', #7058, .T. ) ;
#10972 = VECTOR ( 'NONE', #4893, 1000.000000000000114 ) ;
#10973 = EDGE_CURVE ( 'NONE', #12372, #8058, #11034, .T. ) ;
#10974 = VECTOR ( 'NONE', #3800, 1000.000000000000000 ) ;
#10975 = CARTESIAN_POINT ( 'NONE',  ( -32.50000000000000000, -43.00000000050000182, -137.0552959530000123 ) ) ;
#10976 = EDGE_CURVE ( 'NONE', #9912, #11395, #21777, .T. ) ;
#10977 = CARTESIAN_POINT ( 'NONE',  ( -14.60938321243984106, -44.46164914216203812, -150.0552959529999839 ) ) ;
#10978 = LINE ( 'NONE', #12885, #1927 ) ;
#10979 = ADVANCED_FACE ( 'NONE', ( #7359 ), #14617, .F. ) ;
#10980 = LINE ( 'NONE', #22065, #18461 ) ;
#10981 = EDGE_CURVE ( 'NONE', #1116, #3167, #11603, .T. ) ;
#10982 = DIRECTION ( 'NONE',  ( 1.211690350419999855E-27, 2.765629237170000203E-27, -1.000000000000000000 ) ) ;
#10983 = CARTESIAN_POINT ( 'NONE',  ( -4.500000000000000000, 40.00000000000000000, -150.5552959529999839 ) ) ;
#10984 = CARTESIAN_POINT ( 'NONE',  ( 22.11021350718841560, -15.30096212033725322, -145.5552959529996997 ) ) ;
#10985 = PRODUCT ( 'Latch Lever Guide', 'Latch Lever Guide', '', ( #1501 ) ) ;
#10986 = VECTOR ( 'NONE', #6455, 1000.000000000000000 ) ;
#10987 = CARTESIAN_POINT ( 'NONE',  ( -14.11967125440000004, 36.98834135279999913, -140.5455248810000057 ) ) ;
#10988 = AXIS2_PLACEMENT_3D ( 'NONE', #9830, #15436, #4618 ) ;
#10989 = ORIENTED_EDGE ( 'NONE', *, *, #23347, .F. ) ;
#10990 = VECTOR ( 'NONE', #9937, 1000.000000000000000 ) ;
#10991 = VECTOR ( 'NONE', #4476, 1000.000000000000000 ) ;
#10992 = ORIENTED_EDGE ( 'NONE', *, *, #10708, .T. ) ;
#10993 = AXIS2_PLACEMENT_3D ( 'NONE', #21793, #3813, #3691 ) ;
#10994 = AXIS2_PLACEMENT_3D ( 'NONE', #13433, #13197, #16776 ) ;
#10995 = ORIENTED_EDGE ( 'NONE', *, *, #20300, .F. ) ;
#10996 = CARTESIAN_POINT ( 'NONE',  ( -17.28155659539766731, 34.85587989530459652, -141.0407616605357930 ) ) ;
#10997 = CARTESIAN_POINT ( 'NONE',  ( 3.999999999879999546, -1.500000000000000000, -135.0552959530000123 ) ) ;
#10998 = ORIENTED_EDGE ( 'NONE', *, *, #14269, .F. ) ;
#10999 = DIRECTION ( 'NONE',  ( -0.7633862853691524286, 0.6459422414661292189, 0.000000000000000000 ) ) ;
#11000 = VERTEX_POINT ( 'NONE', #22577 ) ;
#11001 = LINE ( 'NONE', #16140, #20505 ) ;
#11002 = CARTESIAN_POINT ( 'NONE',  ( -19.58178540279576652, 33.51645733664073390, -143.8848924971558176 ) ) ;
#11003 = FACE_OUTER_BOUND ( 'NONE', #20818, .T. ) ;
#11004 = VERTEX_POINT ( 'NONE', #9818 ) ;
#11005 = FACE_OUTER_BOUND ( 'NONE', #18107, .T. ) ;
#11006 = ORIENTED_EDGE ( 'NONE', *, *, #9076, .F. ) ;
#11007 = CARTESIAN_POINT ( 'NONE',  ( 9.101402224069296665, 38.37417018168379457, -141.9668508538656226 ) ) ;
#11008 = EDGE_CURVE ( 'NONE', #3612, #19891, #12581, .T. ) ;
#11009 = VECTOR ( 'NONE', #10736, 1000.000000000000000 ) ;
#11010 =( BOUNDED_SURFACE ( )  B_SPLINE_SURFACE ( 5, 5, ( 
 ( #15079, #22338, #3915, #4367, #20331, #2370 ),
 ( #9702, #9820, #16978, #6033, #4134, #11604 ),
 ( #16746, #459, #7696, #11376, #14965, #18881 ),
 ( #22226, #7922, #15204, #18655, #14727, #5915 ),
 ( #9592, #21995, #18421, #13288, #20558, #22458 ),
 ( #6154, #2592, #223, #5686, #2131, #16624 ),
 ( #3070, #2944, #1046, #8275, #17214, #19360 ),
 ( #815, #10303, #8042, #2715, #11724, #4722 ),
 ( #10178, #8405, #17579, #1294, #17099, #22686 ),
 ( #11967, #17330, #9942, #19231, #6620, #10053 ),
 ( #15321, #12086, #15548, #20791, #22578, #4483 ),
 ( #6381, #15678, #6267, #13518, #8155, #11847 ) ),
 .UNSPECIFIED., .F., .F., .F. ) 
 B_SPLINE_SURFACE_WITH_KNOTS ( ( 6, 3, 3, 6 ),
 ( 6, 6 ),
 ( 0.000000000000000000, 4.371092480729999785, 8.745625541600000830, 13.12578902609999965 ),
 ( 1.570796326521529895, 3.141592653590000062 ),
 .UNSPECIFIED. ) 
 GEOMETRIC_REPRESENTATION_ITEM ( )  RATIONAL_B_SPLINE_SURFACE ( (
 ( 0.2500000000000000000, 0.2499999999651804916, 0.2999999999477704904, 0.3999999999303610054, 0.5999999999303610165, 1.000000000000000000),
 ( 0.2500000000000000000, 0.2499999999651804916, 0.2999999999477704904, 0.3999999999303610054, 0.5999999999303610165, 1.000000000000000000),
 ( 0.2500000000000000000, 0.2499999999651804916, 0.2999999999477704904, 0.3999999999303610054, 0.5999999999303610165, 1.000000000000000000),
 ( 0.2500000000000000000, 0.2499999999651804916, 0.2999999999477704904, 0.3999999999303610054, 0.5999999999303610165, 1.000000000000000000),
 ( 0.2500000000000000000, 0.2499999999651804916, 0.2999999999477704904, 0.3999999999303610054, 0.5999999999303610165, 1.000000000000000000),
 ( 0.2500000000000000000, 0.2499999999651804916, 0.2999999999477704904, 0.3999999999303610054, 0.5999999999303610165, 1.000000000000000000),
 ( 0.2500000000000000000, 0.2499999999651804916, 0.2999999999477704904, 0.3999999999303610054, 0.5999999999303610165, 1.000000000000000000),
 ( 0.2500000000000000000, 0.2499999999651804916, 0.2999999999477704904, 0.3999999999303610054, 0.5999999999303610165, 1.000000000000000000),
 ( 0.2500000000000000000, 0.2499999999651804916, 0.2999999999477704904, 0.3999999999303610054, 0.5999999999303610165, 1.000000000000000000),
 ( 0.2500000000000000000, 0.2499999999651804916, 0.2999999999477704904, 0.3999999999303610054, 0.5999999999303610165, 1.000000000000000000),
 ( 0.2500000000000000000, 0.2499999999651804916, 0.2999999999477704904, 0.3999999999303610054, 0.5999999999303610165, 1.000000000000000000),
 ( 0.2500000000000000000, 0.2499999999651804916, 0.2999999999477704904, 0.3999999999303610054, 0.5999999999303610165, 1.000000000000000000) ) ) 
 REPRESENTATION_ITEM ( '' )  SURFACE ( )  );
#11011 = AXIS2_PLACEMENT_3D ( 'NONE', #2338, #9564, #5650 ) ;
#11012 = CARTESIAN_POINT ( 'NONE',  ( -32.50000000000000000, 12.00000000000000000, -144.0552959529999839 ) ) ;
#11013 = VECTOR ( 'NONE', #11958, 1000.000000000000000 ) ;
#11014 = CIRCLE ( 'NONE', #23191, 0.7500000000000006661 ) ;
#11015 = CARTESIAN_POINT ( 'NONE',  ( -28.18164916493977756, 37.07873981898478633, -148.1638686014308632 ) ) ;
#11016 = ORIENTED_EDGE ( 'NONE', *, *, #5311, .T. ) ;
#11017 = FACE_OUTER_BOUND ( 'NONE', #20476, .T. ) ;
#11018 = VERTEX_POINT ( 'NONE', #17097 ) ;
#11019 = CARTESIAN_POINT ( 'NONE',  ( 8.750000000030000891, -35.98606797749999942, -136.0552959530000123 ) ) ;
#11020 = ORIENTED_EDGE ( 'NONE', *, *, #10109, .F. ) ;
#11021 = CARTESIAN_POINT ( 'NONE',  ( -25.80099178304097762, 37.02638091262101483, -140.6905788942604261 ) ) ;
#11022 = ORIENTED_EDGE ( 'NONE', *, *, #13645, .T. ) ;
#11023 = CARTESIAN_POINT ( 'NONE',  ( -23.01788799736533875, 34.20869732335551561, -140.2024652167382328 ) ) ;
#11024 = CARTESIAN_POINT ( 'NONE',  ( -29.95441468910000182, 40.29796007080000209, -145.3430615500000158 ) ) ;
#11025 = VERTEX_POINT ( 'NONE', #20330 ) ;
#11026 = APPLICATION_PROTOCOL_DEFINITION ( 'draft international standard', 'automotive_design', 1998, #4627 ) ;
#11027 = AXIS2_PLACEMENT_3D ( 'NONE', #18792, #9268, #597 ) ;
#11028 = VECTOR ( 'NONE', #2538, 1000.000000000000000 ) ;
#11029 = ORIENTED_EDGE ( 'NONE', *, *, #10934, .T. ) ;
#11030 = CARTESIAN_POINT ( 'NONE',  ( -25.90907760989742670, 37.01347911741230945, -139.4251635482865765 ) ) ;
#11031 = LINE ( 'NONE', #6790, #2006 ) ;
#11032 = CYLINDRICAL_SURFACE ( 'NONE', #2761, 3.000000000000000000 ) ;
#11033 = CARTESIAN_POINT ( 'NONE',  ( 9.183200060760000838, 0.4999999999990000776, -148.5552959529999839 ) ) ;
#11034 = LINE ( 'NONE', #12820, #22419 ) ;
#11035 = ADVANCED_FACE ( 'NONE', ( #334 ), #458, .T. ) ;
#11036 = CARTESIAN_POINT ( 'NONE',  ( 6.500000000159999125, 28.50000000000000000, -140.5552959529999839 ) ) ;
#11037 = ORIENTED_EDGE ( 'NONE', *, *, #4869, .T. ) ;
#11038 = DIRECTION ( 'NONE',  ( 1.457928428160000110E-12, 1.723197716179999783E-12, -1.000000000000000000 ) ) ;
#11039 = CARTESIAN_POINT ( 'NONE',  ( 8.891031312599221081, 35.55079436630060741, -146.0924816361270189 ) ) ;
#11040 = ORIENTED_EDGE ( 'NONE', *, *, #5300, .T. ) ;
#11041 = AXIS2_PLACEMENT_3D ( 'NONE', #10725, #23473, #3490 ) ;
#11042 = CARTESIAN_POINT ( 'NONE',  ( -8.734077015120000453, -11.22642389220000148, -146.0552959529999839 ) ) ;
#11043 = DIRECTION ( 'NONE',  ( 1.000000000000000000, 2.602084747549999882E-17, 0.000000000000000000 ) ) ;
#11044 = CARTESIAN_POINT ( 'NONE',  ( -16.92892821565927974, 40.42700121177570338, -142.0839162034752121 ) ) ;
#11045 = CARTESIAN_POINT ( 'NONE',  ( -29.31903837101844346, 40.46341529379842683, -142.8387304625044010 ) ) ;
#11046 = VERTEX_POINT ( 'NONE', #22337 ) ;
#11047 = CARTESIAN_POINT ( 'NONE',  ( -6.812760379890000273, 32.88798608609999974, -143.6676051400000063 ) ) ;
#11048 = CARTESIAN_POINT ( 'NONE',  ( 10.68320006080000084, -19.50000000000000000, -138.5552959529999839 ) ) ;
#11049 = FACE_OUTER_BOUND ( 'NONE', #8837, .T. ) ;
#11050 = CARTESIAN_POINT ( 'NONE',  ( 27.18320006080000084, 0.9999999999989999111, -150.0552959529999839 ) ) ;
#11051 = DIRECTION ( 'NONE',  ( 1.000000000000000000, 0.000000000000000000, 2.516505522483685870E-12 ) ) ;
#11052 = CARTESIAN_POINT ( 'NONE',  ( 19.34345092960000301, -49.66753540199999151, -149.5552959529999839 ) ) ;
#11053 = ORIENTED_EDGE ( 'NONE', *, *, #13454, .T. ) ;
#11054 = CARTESIAN_POINT ( 'NONE',  ( -27.58110728285923940, 34.24318910288427986, -147.7245096245594027 ) ) ;
#11055 = CARTESIAN_POINT ( 'NONE',  ( 13.13369214870000157, 50.50000000000000000, -136.0552959530000123 ) ) ;
#11056 = CYLINDRICAL_SURFACE ( 'NONE', #17836, 35.00000000000000000 ) ;
#11057 = CARTESIAN_POINT ( 'NONE',  ( -5.872912812989576459, 37.83051333333958155, -148.3065483569547780 ) ) ;
#11058 = DIRECTION ( 'NONE',  ( 2.839308199620000013E-14, 3.568879590630000244E-13, 1.000000000000000000 ) ) ;
#11059 = CLOSED_SHELL ( 'NONE', ( #17619, #6190, #12682, #9916, #19715, #22499, #22321, #18990, #1210, #22927 ) ) ;
#11060 = ORIENTED_EDGE ( 'NONE', *, *, #18981, .T. ) ;
#11061 = ADVANCED_FACE ( 'NONE', ( #8040 ), #11254, .F. ) ;
#11062 = CARTESIAN_POINT ( 'NONE',  ( -26.68542098469999857, 39.18140699330000132, -140.9632721460000084 ) ) ;
#11063 = DIRECTION ( 'NONE',  ( -2.602084704489999637E-17, 1.000000000000000000, 0.000000000000000000 ) ) ;
#11064 = EDGE_CURVE ( 'NONE', #19530, #18104, #16977, .T. ) ;
#11065 = ORIENTED_EDGE ( 'NONE', *, *, #11527, .T. ) ;
#11066 = B_SPLINE_CURVE_WITH_KNOTS ( 'NONE', 1,
 ( #9549, #11208 ),
 .UNSPECIFIED., .F., .F.,
 ( 2, 2 ),
 ( -6.000000000000000000, 6.000000000000000000 ),
 .UNSPECIFIED. ) ;
#11067 = ORIENTED_EDGE ( 'NONE', *, *, #22118, .F. ) ;
#11068 = CARTESIAN_POINT ( 'NONE',  ( 4.890679856720475449, -2.038243779785305687, -136.0552959530110684 ) ) ;
#11069 = CARTESIAN_POINT ( 'NONE',  ( -32.50000000000000000, 0.9999999999959999775, -132.5552959530000123 ) ) ;
#11070 = FACE_OUTER_BOUND ( 'NONE', #20981, .T. ) ;
#11071 = DIRECTION ( 'NONE',  ( 0.4108698089121693986, -0.9116940276893763517, 3.145631903104610871E-13 ) ) ;
#11072 = ORIENTED_EDGE ( 'NONE', *, *, #22608, .F. ) ;
#11073 = VECTOR ( 'NONE', #10806, 1000.000000000000000 ) ;
#11074 = AXIS2_PLACEMENT_3D ( 'NONE', #14088, #10844, #8944 ) ;
#11075 = CARTESIAN_POINT ( 'NONE',  ( -19.39325354300213533, 37.07505107993059568, -139.9601895477539131 ) ) ;
#11076 = VECTOR ( 'NONE', #7725, 1000.000000000000000 ) ;
#11077 = DIRECTION ( 'NONE',  ( 1.000000000000000000, 0.000000000000000000, 0.000000000000000000 ) ) ;
#11078 = DIRECTION ( 'NONE',  ( 0.000000000000000000, -1.000000000000000000, 8.159623473500000156E-13 ) ) ;
#11079 = DIRECTION ( 'NONE',  ( -5.094701932209999624E-24, -1.000000000000000000, 1.149947916579999802E-35 ) ) ;
#11080 = CARTESIAN_POINT ( 'NONE',  ( 32.50000000000000000, -27.03620104879999886, -137.0552959530000123 ) ) ;
#11081 = EDGE_CURVE ( 'NONE', #16174, #7366, #13516, .T. ) ;
#11082 = FACE_OUTER_BOUND ( 'NONE', #12332, .T. ) ;
#11083 = PLANE ( 'NONE',  #12216 ) ;
#11084 = DIRECTION ( 'NONE',  ( 1.526468026909999897E-13, 8.159623473500000156E-13, 1.000000000000000000 ) ) ;
#11085 = VERTEX_POINT ( 'NONE', #4023 ) ;
#11086 = CARTESIAN_POINT ( 'NONE',  ( -6.389646268321180322, 36.98420143700543861, -147.3954793911336481 ) ) ;
#11087 = VECTOR ( 'NONE', #16040, 1000.000000000000227 ) ;
#11088 = AXIS2_PLACEMENT_3D ( 'NONE', #23220, #1338, #14290 ) ;
#11089 = VERTEX_POINT ( 'NONE', #2369 ) ;
#11090 = VECTOR ( 'NONE', #7806, 1000.000000000000000 ) ;
#11091 = CARTESIAN_POINT ( 'NONE',  ( -7.500000000000000000, 48.50000000000000000, -150.0552959529999839 ) ) ;
#11092 = LINE ( 'NONE', #18259, #18225 ) ;
#11093 = CARTESIAN_POINT ( 'NONE',  ( -15.19857565924485421, -44.49993277009840398, -150.0552959529999839 ) ) ;
#11094 = CARTESIAN_POINT ( 'NONE',  ( 10.68320006080000084, -20.50000000000000000, -150.0552959529999839 ) ) ;
#11095 = CARTESIAN_POINT ( 'NONE',  ( -13.05391057859098325, 32.94097121706953857, -141.8088358606670454 ) ) ;
#11096 = CARTESIAN_POINT ( 'NONE',  ( -32.50000000000000000, 49.50000000000000000, -137.0552959530000123 ) ) ;
#11097 = EDGE_CURVE ( 'NONE', #1062, #17719, #22225, .T. ) ;
#11098 = CARTESIAN_POINT ( 'NONE',  ( 8.750000000000000000, -47.00000000000000000, -150.5552959529999839 ) ) ;
#11099 = DIRECTION ( 'NONE',  ( -0.1297261684090585954, 0.9915498581664488054, 1.179599313710532933E-12 ) ) ;
#11100 = DIRECTION ( 'NONE',  ( 2.257144641399999941E-12, -4.009147065140000298E-51, 1.000000000000000000 ) ) ;
#11101 = DIRECTION ( 'NONE',  ( 0.000000000000000000, 1.000000000000000000, 0.000000000000000000 ) ) ;
#11102 = VERTEX_POINT ( 'NONE', #20673 ) ;
#11103 = STYLED_ITEM ( 'NONE', ( #541 ), #10046 ) ;
#11104 = UNCERTAINTY_MEASURE_WITH_UNIT (LENGTH_MEASURE( 1.000000000000000082E-05 ), #23502, 'distance_accuracy_value', 'NONE');
#11105 = VECTOR ( 'NONE', #6215, 1000.000000000000000 ) ;
#11106 = ORIENTED_EDGE ( 'NONE', *, *, #1695, .F. ) ;
#11107 = ADVANCED_FACE ( 'NONE', ( #11491 ), #818, .F. ) ;
#11108 = EDGE_CURVE ( 'NONE', #17890, #6188, #12085, .T. ) ;
#11109 = ORIENTED_EDGE ( 'NONE', *, *, #18269, .F. ) ;
#11110 = CARTESIAN_POINT ( 'NONE',  ( 8.500000000050000892, 37.00000000000000000, -146.5552959529999839 ) ) ;
#11111 = DIRECTION ( 'NONE',  ( 0.6459422414661314393, 0.7633862853691505412, 0.000000000000000000 ) ) ;
#11112 = DIRECTION ( 'NONE',  ( 0.000000000000000000, -1.000000000000000000, 0.000000000000000000 ) ) ;
#11113 = EDGE_CURVE ( 'NONE', #8089, #18676, #10177, .T. ) ;
#11114 = VERTEX_POINT ( 'NONE', #4607 ) ;
#11115 = CARTESIAN_POINT ( 'NONE',  ( 25.42349012529465924, 35.71905350742473928, -136.0552959530573673 ) ) ;
#11116 = EDGE_CURVE ( 'NONE', #19064, #17007, #11846, .T. ) ;
#11117 = CARTESIAN_POINT ( 'NONE',  ( -20.10690122708593108, 36.24603085032271110, -140.7204002581620728 ) ) ;
#11118 = DIRECTION ( 'NONE',  ( 1.000000000000000000, 0.000000000000000000, 0.000000000000000000 ) ) ;
#11119 = EDGE_LOOP ( 'NONE', ( #3195, #17715, #16625, #11398, #3687 ) ) ;
#11120 = CARTESIAN_POINT ( 'NONE',  ( 12.49750131802634989, 15.89089960018812775, -136.0552959530134842 ) ) ;
#11121 = DIRECTION ( 'NONE',  ( 2.257157423930000049E-12, 0.000000000000000000, 1.000000000000000000 ) ) ;
#11122 = CARTESIAN_POINT ( 'NONE',  ( -17.89449577229859401, 36.92509720026601627, -147.9522036891449943 ) ) ;
#11123 = FACE_OUTER_BOUND ( 'NONE', #7501, .T. ) ;
#11124 = ORIENTED_EDGE ( 'NONE', *, *, #11837, .F. ) ;
#11125 = EDGE_CURVE ( 'NONE', #18387, #5495, #2822, .T. ) ;
#11126 = CARTESIAN_POINT ( 'NONE',  ( -4.499999999929999994, 34.00000000000000000, -138.0552959530000123 ) ) ;
#11127 = ORIENTED_EDGE ( 'NONE', *, *, #3740, .T. ) ;
#11128 = DIRECTION ( 'NONE',  ( 2.257749542879999954E-12, 0.000000000000000000, 1.000000000000000000 ) ) ;
#11129 = ORIENTED_EDGE ( 'NONE', *, *, #7770, .T. ) ;
#11130 = CARTESIAN_POINT ( 'NONE',  ( -25.93177281299394465, 40.35538820219090894, -142.1683974516384410 ) ) ;
#11131 = EDGE_CURVE ( 'NONE', #15988, #18172, #1045, .T. ) ;
#11132 = ORIENTED_EDGE ( 'NONE', *, *, #14085, .F. ) ;
#11133 = CARTESIAN_POINT ( 'NONE',  ( -22.56584646715587539, 37.05444931714286838, -139.6092474954658940 ) ) ;
#11134 = ADVANCED_FACE ( 'NONE', ( #4721 ), #11965, .F. ) ;
#11135 = ORIENTED_EDGE ( 'NONE', *, *, #11097, .T. ) ;
#11136 = FACE_OUTER_BOUND ( 'NONE', #13606, .T. ) ;
#11137 = DIRECTION ( 'NONE',  ( 0.000000000000000000, 1.000000000000000000, 0.000000000000000000 ) ) ;
#11138 = ORIENTED_EDGE ( 'NONE', *, *, #15760, .F. ) ;
#11139 =( NAMED_UNIT ( * ) SI_UNIT ( $, .STERADIAN. ) SOLID_ANGLE_UNIT ( ) );
#11140 = VERTEX_POINT ( 'NONE', #21626 ) ;
#11141 = VECTOR ( 'NONE', #22543, 1000.000000000000000 ) ;
#11142 = DIRECTION ( 'NONE',  ( 1.000000000000000000, 0.000000000000000000, 0.000000000000000000 ) ) ;
#11143 = CARTESIAN_POINT ( 'NONE',  ( -34.50000000000000000, 13.04114892279999971, -145.8104610769999852 ) ) ;
#11144 = DIRECTION ( 'NONE',  ( 0.000000000000000000, -2.257144641399999941E-12, -1.000000000000000000 ) ) ;
#11145 = DIRECTION ( 'NONE',  ( 0.000000000000000000, -4.148443855749999753E-27, -1.000000000000000000 ) ) ;
#11146 =( BOUNDED_CURVE ( )  B_SPLINE_CURVE ( 5, ( #7676, #9570, #11015, #2003, #16846, #18292 ),
 .UNSPECIFIED., .F., .F. ) 
 B_SPLINE_CURVE_WITH_KNOTS ( ( 6, 6 ),
 ( 0.000000000000000000, 1.570796326695737877 ),
 .UNSPECIFIED. ) 
 CURVE ( )  GEOMETRIC_REPRESENTATION_ITEM ( )  RATIONAL_B_SPLINE_CURVE ( ( 1.000000000000000000, 0.6000000000252768695, 0.4000000000252768584, 0.3000000000189576577, 0.2500000000126384458, 0.2500000000000000000 ) ) 
 REPRESENTATION_ITEM ( '' )  );
#11147 = CARTESIAN_POINT ( 'NONE',  ( -10.43323856990612875, 37.07027821888497954, -139.9576636760149313 ) ) ;
#11148 = LINE ( 'NONE', #20674, #6787 ) ;
#11149 = ORIENTED_EDGE ( 'NONE', *, *, #11430, .F. ) ;
#11150 = DIRECTION ( 'NONE',  ( 1.701177084980000217E-20, 4.426606872460000157E-37, 1.000000000000000000 ) ) ;
#11151 = DIRECTION ( 'NONE',  ( 1.211690350419999855E-27, 2.765629237170000203E-27, -1.000000000000000000 ) ) ;
#11152 = ORIENTED_EDGE ( 'NONE', *, *, #10257, .F. ) ;
#11153 = CARTESIAN_POINT ( 'NONE',  ( 3.742764529247745386, -4.809518488836389771, -150.0552959529999839 ) ) ;
#11154 = CARTESIAN_POINT ( 'NONE',  ( -11.19806794730000021, 41.07225940149999843, -141.8826665010000170 ) ) ;
#11155 = VECTOR ( 'NONE', #13460, 1000.000000000000000 ) ;
#11156 = CARTESIAN_POINT ( 'NONE',  ( -16.54806230416816959, 38.77190534598552318, -140.1780706808168588 ) ) ;
#11157 = CARTESIAN_POINT ( 'NONE',  ( -29.62343099156833759, 40.28042712731500785, -145.3785591165033679 ) ) ;
#11158 = ORIENTED_EDGE ( 'NONE', *, *, #17277, .F. ) ;
#11159 = SURFACE_STYLE_USAGE ( .BOTH. , #7593 ) ;
#11160 = CARTESIAN_POINT ( 'NONE',  ( -25.80099178328665488, 37.02638091259170494, -140.6905788942244158 ) ) ;
#11161 = ORIENTED_EDGE ( 'NONE', *, *, #5188, .T. ) ;
#11162 = DIRECTION ( 'NONE',  ( 4.510774274160000731E-12, -1.321907670990000086E-13, 1.000000000000000000 ) ) ;
#11163 = CARTESIAN_POINT ( 'NONE',  ( -21.35824191589999899, -32.00000000000000000, -146.2257682199999920 ) ) ;
#11164 = EDGE_CURVE ( 'NONE', #15695, #1359, #16488, .T. ) ;
#11165 = CARTESIAN_POINT ( 'NONE',  ( -6.334350183781824128, -17.33929910105837990, -144.5552959530011208 ) ) ;
#11166 = EDGE_CURVE ( 'NONE', #22352, #3173, #194, .T. ) ;
#11167 = CARTESIAN_POINT ( 'NONE',  ( -19.59722155829454593, 38.81238647146790299, -140.2173786323916715 ) ) ;
#11168 = ORIENTED_EDGE ( 'NONE', *, *, #1266, .F. ) ;
#11169 = CARTESIAN_POINT ( 'NONE',  ( -27.78250035523632988, 34.89932656597451199, -146.8789310658169427 ) ) ;
#11170 = CARTESIAN_POINT ( 'NONE',  ( -12.50000000000000000, 42.50000000000000000, -150.0552959529999839 ) ) ;
#11171 = DIRECTION ( 'NONE',  ( -1.000000000000000000, 0.000000000000000000, 0.000000000000000000 ) ) ;
#11172 = CARTESIAN_POINT ( 'NONE',  ( 22.33963087269999903, -30.94765732060000119, -147.5552959529999839 ) ) ;
#11173 = CARTESIAN_POINT ( 'NONE',  ( -21.74973190997082284, -4.669170177705934677, -146.3157682190010007 ) ) ;
#11174 = ORIENTED_EDGE ( 'NONE', *, *, #2702, .T. ) ;
#11175 = VECTOR ( 'NONE', #11905, 999.9999999999998863 ) ;
#11176 = CARTESIAN_POINT ( 'NONE',  ( -2.499999999859999988, 41.50000000000000000, -146.5552959529999839 ) ) ;
#11177 = CARTESIAN_POINT ( 'NONE',  ( -16.20113092416073997, -43.92022845431750966, -136.0552959529634336 ) ) ;
#11178 = ORIENTED_EDGE ( 'NONE', *, *, #2562, .T. ) ;
#11179 = ORIENTED_EDGE ( 'NONE', *, *, #10824, .T. ) ;
#11180 = CARTESIAN_POINT ( 'NONE',  ( -9.434278515689999978, -18.41834002140000237, -147.5552959529999839 ) ) ;
#11181 = CARTESIAN_POINT ( 'NONE',  ( -29.29455083632570123, 36.96746664035849506, -139.4767999530270117 ) ) ;
#11182 = CARTESIAN_POINT ( 'NONE',  ( 25.15155135439999867, -26.08415009650000016, -146.5552959529999839 ) ) ;
#11183 = CARTESIAN_POINT ( 'NONE',  ( 32.00000000000000000, 20.96379895120000114, -136.0552959530000123 ) ) ;
#11184 = ORIENTED_EDGE ( 'NONE', *, *, #1525, .T. ) ;
#11185 = DIRECTION ( 'NONE',  ( -0.9848077530125619594, 0.000000000000000000, -0.1736481776649230202 ) ) ;
#11186 = CARTESIAN_POINT ( 'NONE',  ( -18.42369010557010967, 35.12722143684463560, -148.4184552812508571 ) ) ;
#11187 = CARTESIAN_POINT ( 'NONE',  ( -32.50000000000000000, 67.50000000000000000, -144.0552959529999839 ) ) ;
#11188 = DIRECTION ( 'NONE',  ( -0.7071067811865475727, -0.7071067811865475727, 0.000000000000000000 ) ) ;
#11189 = EDGE_CURVE ( 'NONE', #2513, #7104, #5187, .T. ) ;
#11190 = CARTESIAN_POINT ( 'NONE',  ( -24.53283754947133488, 37.97921577274999549, -148.7308746522571141 ) ) ;
#11191 = VECTOR ( 'NONE', #17558, 1000.000000000000000 ) ;
#11192 = EDGE_CURVE ( 'NONE', #15113, #5364, #12792, .T. ) ;
#11193 = CARTESIAN_POINT ( 'NONE',  ( 9.709183429561321077, -20.23902802861211114, -148.5552959530000123 ) ) ;
#11194 = DIRECTION ( 'NONE',  ( -0.000000000000000000, 1.000000000000000000, 0.000000000000000000 ) ) ;
#11195 = DIRECTION ( 'NONE',  ( 0.000000000000000000, 0.000000000000000000, 1.000000000000000000 ) ) ;
#11196 = LINE ( 'NONE', #22278, #19555 ) ;
#11197 = ORIENTED_EDGE ( 'NONE', *, *, #15071, .T. ) ;
#11198 = CARTESIAN_POINT ( 'NONE',  ( -5.659867863817344080, 38.70771930248351822, -140.0293976191753984 ) ) ;
#11199 = ORIENTED_EDGE ( 'NONE', *, *, #4351, .T. ) ;
#11200 = FILL_AREA_STYLE ('',( #21944 ) ) ;
#11202 = VECTOR ( 'NONE', #17618, 1000.000000000000227 ) ;
#11201 = CARTESIAN_POINT ( 'NONE',  ( -21.33871772388139831, 34.54066873246879510, -147.2646375964223751 ) ) ;
#11203 = DIRECTION ( 'NONE',  ( 1.000000000000000000, 0.000000000000000000, 0.000000000000000000 ) ) ;
#11204 = ORIENTED_EDGE ( 'NONE', *, *, #8066, .T. ) ;
#11205 = CARTESIAN_POINT ( 'NONE',  ( -13.20169807812806084, 35.46390522416190549, -140.5417041917768302 ) ) ;
#11206 = CARTESIAN_POINT ( 'NONE',  ( 1.133692148650000009, -50.50000000000000000, -137.0552959530000123 ) ) ;
#11207 = CARTESIAN_POINT ( 'NONE',  ( -35.47299999999999898, 14.00000000000000000, -144.5552959529999839 ) ) ;
#11208 = CARTESIAN_POINT ( 'NONE',  ( 13.13369214859999978, 50.50000000000000000, -137.0552959530000123 ) ) ;
#11209 = CARTESIAN_POINT ( 'NONE',  ( -16.50000000000000000, -43.00000000000000000, -150.0552959529999839 ) ) ;
#11210 = CARTESIAN_POINT ( 'NONE',  ( 3.000000000010000001, -3.699232232950709243, -136.0552959530068051 ) ) ;
#11211 = ORIENTED_EDGE ( 'NONE', *, *, #6762, .F. ) ;
#11212 = ADVANCED_FACE ( 'NONE', ( #18046, #18162, #23518, #7437, #8979, #21968, #5654, #3405, #10882, #9098, #1757, #3291 ), #9218, .F. ) ;
#11213 = DIRECTION ( 'NONE',  ( -2.507771768022264771E-12, -1.592655090489709912E-17, 1.000000000000000000 ) ) ;
#11214 = ORIENTED_EDGE ( 'NONE', *, *, #4674, .F. ) ;
#11215 = ORIENTED_EDGE ( 'NONE', *, *, #2645, .F. ) ;
#11216 = AXIS2_PLACEMENT_3D ( 'NONE', #19244, #10190, #1188 ) ;
#11217 = PLANE ( 'NONE',  #6124 ) ;
#11218 = CARTESIAN_POINT ( 'NONE',  ( 12.50000000010000001, 16.89444872450000190, -143.5552959529999839 ) ) ;
#11219 = VECTOR ( 'NONE', #14573, 1000.000000000000000 ) ;
#11220 = CARTESIAN_POINT ( 'NONE',  ( 10.25767361208684036, 27.00937110138498909, -136.0552959530231760 ) ) ;
#11221 = ORIENTED_EDGE ( 'NONE', *, *, #3206, .T. ) ;
#11222 = LINE ( 'NONE', #20647, #15590 ) ;
#11223 = ADVANCED_FACE ( 'NONE', ( #11005 ), #10648, .T. ) ;
#11224 = FACE_OUTER_BOUND ( 'NONE', #23479, .T. ) ;
#11225 = LINE ( 'NONE', #16486, #17806 ) ;
#11226 = ORIENTED_EDGE ( 'NONE', *, *, #8353, .F. ) ;
#11227 = CARTESIAN_POINT ( 'NONE',  ( -21.40986708713248632, 40.96636350904213231, -144.4750854696517877 ) ) ;
#11228 = CARTESIAN_POINT ( 'NONE',  ( 9.961649902054594108, 37.34070208382173917, -141.5783375515752311 ) ) ;
#11229 = ADVANCED_FACE ( 'NONE', ( #18287 ), #17803, .F. ) ;
#11230 = CARTESIAN_POINT ( 'NONE',  ( -7.010349701930000066, 37.05829245179999987, -148.1453878979999956 ) ) ;
#11231 = AXIS2_PLACEMENT_3D ( 'NONE', #9192, #14451, #170 ) ;
#11232 = VECTOR ( 'NONE', #9547, 1000.000000000000000 ) ;
#11233 = VERTEX_POINT ( 'NONE', #12679 ) ;
#11234 = PLANE ( 'NONE',  #6501 ) ;
#11235 = VERTEX_POINT ( 'NONE', #16263 ) ;
#11236 = PLANE ( 'NONE',  #4490 ) ;
#11237 = EDGE_CURVE ( 'NONE', #2622, #17961, #5351, .T. ) ;
#11238 = ORIENTED_EDGE ( 'NONE', *, *, #20022, .F. ) ;
#11239 = CARTESIAN_POINT ( 'NONE',  ( -26.95224972473072000, 39.68365438105159626, -147.7577323695496148 ) ) ;
#11240 = VERTEX_POINT ( 'NONE', #14241 ) ;
#11241 = CARTESIAN_POINT ( 'NONE',  ( -23.03288344411683752, 33.05775148879286718, -141.7732690776623485 ) ) ;
#11242 = VERTEX_POINT ( 'NONE', #3533 ) ;
#11243 = CARTESIAN_POINT ( 'NONE',  ( -13.15635984007524684, -45.39900052719453782, -150.0552959530000123 ) ) ;
#11244 = ORIENTED_EDGE ( 'NONE', *, *, #18983, .F. ) ;
#11245 = SHAPE_DEFINITION_REPRESENTATION ( #12416, #2821 ) ;
#11246 = VERTEX_POINT ( 'NONE', #21505 ) ;
#11247 = CARTESIAN_POINT ( 'NONE',  ( -29.62827070406144969, 36.92763176543196124, -139.7399851634201582 ) ) ;
#11248 = ADVANCED_FACE ( 'NONE', ( #17929 ), #21860, .F. ) ;
#11249 = PLANE ( 'NONE',  #9843 ) ;
#11250 = VECTOR ( 'NONE', #19578, 1000.000000000000000 ) ;
#11251 = CARTESIAN_POINT ( 'NONE',  ( -4.888913597060000171, -24.24628707910000003, -143.5552959529999839 ) ) ;
#11252 = DIRECTION ( 'NONE',  ( -0.1435602414469281940, -0.9896415801065048257, 3.849849731938073961E-13 ) ) ;
#11253 = ADVANCED_FACE ( 'NONE', ( #8867 ), #23399, .T. ) ;
#11254 = PLANE ( 'NONE',  #9121 ) ;
#11255 = LINE ( 'NONE', #13170, #9047 ) ;
#11256 = ORIENTED_EDGE ( 'NONE', *, *, #10432, .T. ) ;
#11257 = CARTESIAN_POINT ( 'NONE',  ( -34.50000000000000000, 48.00000000000000000, -150.5552959529999839 ) ) ;
#11258 = EDGE_CURVE ( 'NONE', #22422, #7225, #7331, .T. ) ;
#11259 = DIRECTION ( 'NONE',  ( 1.000000000000000000, 0.000000000000000000, 0.000000000000000000 ) ) ;
#11260 = EDGE_CURVE ( 'NONE', #17461, #4448, #12284, .T. ) ;
#11261 = ORIENTED_EDGE ( 'NONE', *, *, #15648, .T. ) ;
#11262 = LINE ( 'NONE', #20227, #3309 ) ;
#11263 = EDGE_CURVE ( 'NONE', #10478, #6817, #13257, .T. ) ;
#11264 = AXIS2_PLACEMENT_3D ( 'NONE', #2462, #3770, #435 ) ;
#11265 = CARTESIAN_POINT ( 'NONE',  ( -13.08363943609140989, 37.92745778430769121, -148.2189490109368535 ) ) ;
#11266 = ADVANCED_FACE ( 'NONE', ( #9789 ), #2348, .F. ) ;
#11267 = CARTESIAN_POINT ( 'NONE',  ( -16.35051094564224172, 37.08015310165124134, -139.9332297720636973 ) ) ;
#11268 = CARTESIAN_POINT ( 'NONE',  ( -29.38682351424920114, 41.54928687793172060, -144.4052646031983898 ) ) ;
#11269 = VECTOR ( 'NONE', #18605, 1000.000000000000227 ) ;
#11270 = ORIENTED_EDGE ( 'NONE', *, *, #13746, .F. ) ;
#11271 = DIRECTION ( 'NONE',  ( 1.000000000000000000, 0.000000000000000000, 0.000000000000000000 ) ) ;
#11272 = DIRECTION ( 'NONE',  ( 0.000000000000000000, 1.000000000000000000, 0.000000000000000000 ) ) ;
#11273 = ORIENTED_EDGE ( 'NONE', *, *, #11810, .F. ) ;
#11274 = CARTESIAN_POINT ( 'NONE',  ( -4.499999999919999105, 37.00000000000000000, -135.0552959530000123 ) ) ;
#11275 = CARTESIAN_POINT ( 'NONE',  ( -38.72222222220000276, 47.50000000000000000, -140.5552959529999839 ) ) ;
#11276 = DIRECTION ( 'NONE',  ( -1.000000000000000000, 0.000000000000000000, 0.000000000000000000 ) ) ;
#11277 = CARTESIAN_POINT ( 'NONE',  ( -21.50444101780000139, 40.78041997809999941, -146.2395182369999986 ) ) ;
#11278 = VERTEX_POINT ( 'NONE', #1370 ) ;
#11279 =( BOUNDED_CURVE ( )  B_SPLINE_CURVE ( 5, ( #21178, #22960, #13799, #19257, #6644, #2970, #13905, #3200, #10434, #21294, #3091, #23073 ),
 .UNSPECIFIED., .F., .F. ) 
 B_SPLINE_CURVE_WITH_KNOTS ( ( 6, 3, 3, 6 ),
 ( 0.000000000000000000, 4.398006073320000375, 8.633600727160001043, 12.71824907600000110 ),
 .UNSPECIFIED. ) 
 CURVE ( )  GEOMETRIC_REPRESENTATION_ITEM ( )  RATIONAL_B_SPLINE_CURVE ( ( 0.2500000000000000000, 0.2500000000000000000, 0.2500000000000000000, 0.2500000000000000000, 0.2500000000000000000, 0.2500000000000000000, 0.2500000000000000000, 0.2500000000000000000, 0.2500000000000000000, 0.2500000000000000000, 0.2500000000000000000, 0.2500000000000000000 ) ) 
 REPRESENTATION_ITEM ( '' )  );
#11280 = CARTESIAN_POINT ( 'NONE',  ( -34.50000000000000000, 28.00000000000000000, -141.5552959529999839 ) ) ;
#11281 = VERTEX_POINT ( 'NONE', #11937 ) ;
#11282 = CARTESIAN_POINT ( 'NONE',  ( -9.347107914279998653, -17.32706600430000066, -143.5552959529999839 ) ) ;
#11283 = PLANE ( 'NONE',  #7305 ) ;
#11284 = CARTESIAN_POINT ( 'NONE',  ( -5.449266527167752727, 43.97928331370520993, -136.0552959529877342 ) ) ;
#11285 = AXIS2_PLACEMENT_3D ( 'NONE', #23350, #15848, #14302 ) ;
#11286 = ORIENTED_EDGE ( 'NONE', *, *, #21641, .T. ) ;
#11287 = CARTESIAN_POINT ( 'NONE',  ( 10.81534092360039701, -19.49999999999999645, -148.5552959529999839 ) ) ;
#11288 = AXIS2_PLACEMENT_3D ( 'NONE', #15740, #14076, #21106 ) ;
#11289 = LINE ( 'NONE', #15353, #13605 ) ;
#11290 = ORIENTED_EDGE ( 'NONE', *, *, #5613, .F. ) ;
#11291 = ADVANCED_FACE ( 'NONE', ( #20886 ), #19203, .F. ) ;
#11292 = ORIENTED_EDGE ( 'NONE', *, *, #7650, .F. ) ;
#11293 = DIRECTION ( 'NONE',  ( 0.000000000000000000, 1.000000000000000000, 0.000000000000000000 ) ) ;
#11294 = CARTESIAN_POINT ( 'NONE',  ( 29.68320006080000084, -16.50000000000000000, -150.0552959529999839 ) ) ;
#11295 = B_SPLINE_CURVE_WITH_KNOTS ( 'NONE', 3,
 ( #697, #8922, #4144, #21692, #18106, #22464, #6160, #13410, #18228, #5377 ),
 .UNSPECIFIED., .F., .F.,
 ( 4, 2, 2, 2, 4 ),
 ( 0.000000000000000000, 0.2500000000000001110, 0.5000000000000002220, 0.7500000000000003331, 1.000000000000000000 ),
 .UNSPECIFIED. ) ;
#11296 = DIRECTION ( 'NONE',  ( -1.000000000000000000, 0.000000000000000000, 2.257144641399999941E-12 ) ) ;
#11297 = CARTESIAN_POINT ( 'NONE',  ( 7.406798920894477334, 35.97274762639648316, -141.7760678467019204 ) ) ;
#11298 = VERTEX_POINT ( 'NONE', #8130 ) ;
#11299 = FACE_OUTER_BOUND ( 'NONE', #7227, .T. ) ;
#11300 = CARTESIAN_POINT ( 'NONE',  ( -18.07392865170000107, -34.50000000000000000, -146.3157682190000060 ) ) ;
#11301 = AXIS2_PLACEMENT_3D ( 'NONE', #11187, #11302, #20147 ) ;
#11302 = DIRECTION ( 'NONE',  ( 1.000000000000000000, 2.602084704489999637E-17, -1.701177084830000066E-20 ) ) ;
#11303 = DIRECTION ( 'NONE',  ( 1.701177084980000217E-20, 4.426606872460000157E-37, 1.000000000000000000 ) ) ;
#11304 = CARTESIAN_POINT ( 'NONE',  ( -23.45607911474452933, 41.63247930368797967, -144.6595350281507706 ) ) ;
#11305 = VECTOR ( 'NONE', #6166, 1000.000000000000000 ) ;
#11306 = CARTESIAN_POINT ( 'NONE',  ( -15.27594358124297536, 35.39499320739097499, -147.3719605119253799 ) ) ;
#11307 = CARTESIAN_POINT ( 'NONE',  ( -19.04867772230000256, 35.29145880730000329, -148.2212826610000036 ) ) ;
#11308 = CARTESIAN_POINT ( 'NONE',  ( 31.50000000000000000, 40.03620104880000241, -150.0552959529999839 ) ) ;
#11309 = DIRECTION ( 'NONE',  ( -1.000000000000000000, 0.000000000000000000, 0.000000000000000000 ) ) ;
#11310 = ORIENTED_EDGE ( 'NONE', *, *, #11260, .F. ) ;
#11311 = CARTESIAN_POINT ( 'NONE',  ( -6.414293125256102179, 40.89447441809702610, -144.3648767483412598 ) ) ;
#11312 = FACE_BOUND ( 'NONE', #12145, .T. ) ;
#11313 = EDGE_CURVE ( 'NONE', #16877, #968, #21241, .T. ) ;
#11314 = ORIENTED_EDGE ( 'NONE', *, *, #20251, .F. ) ;
#11315 = LINE ( 'NONE', #18368, #4214 ) ;
#11316 = AXIS2_PLACEMENT_3D ( 'NONE', #2163, #11523, #7958 ) ;
#11317 = ADVANCED_FACE ( 'NONE', ( #13856 ), #2916, .T. ) ;
#11318 = CARTESIAN_POINT ( 'NONE',  ( -23.02519999780000148, 33.35976406540000028, -141.9520978260000277 ) ) ;
#11319 = DIRECTION ( 'NONE',  ( -1.526468026909999897E-13, -8.159623473500000156E-13, -1.000000000000000000 ) ) ;
#11320 = ORIENTED_EDGE ( 'NONE', *, *, #5575, .T. ) ;
#11321 = CARTESIAN_POINT ( 'NONE',  ( -12.84285234542676690, 33.24967124346566294, -141.9488202108821326 ) ) ;
#11322 = CARTESIAN_POINT ( 'NONE',  ( -25.35824191590000254, -18.00000000000000000, -146.3157682190000060 ) ) ;
#11323 = DIRECTION ( 'NONE',  ( 0.000000000000000000, -1.000000000000000000, 0.000000000000000000 ) ) ;
#11324 = DIRECTION ( 'NONE',  ( 0.000000000000000000, 0.000000000000000000, 1.000000000000000000 ) ) ;
#11325 = CARTESIAN_POINT ( 'NONE',  ( 24.59017985859999911, -26.91621017459999976, -148.5552959529999839 ) ) ;
#11326 = DIRECTION ( 'NONE',  ( 4.511946372079999833E-12, -1.278976924369999890E-13, 1.000000000000000000 ) ) ;
#11327 = EDGE_LOOP ( 'NONE', ( #5892, #1035, #23152, #5659 ) ) ;
#11328 = CARTESIAN_POINT ( 'NONE',  ( -28.54444076201625435, 32.93521038166499437, -146.4073461492294541 ) ) ;
#11330 = VERTEX_POINT ( 'NONE', #12181 ) ;
#11329 = VECTOR ( 'NONE', #577, 1000.000000000000000 ) ;
#11331 = VECTOR ( 'NONE', #10453, 1000.000000000000114 ) ;
#11332 = ORIENTED_EDGE ( 'NONE', *, *, #17549, .F. ) ;
#11333 = CARTESIAN_POINT ( 'NONE',  ( -14.02654126840723592, 33.59767434680839671, -142.2851935300912771 ) ) ;
#11334 = DIRECTION ( 'NONE',  ( 0.000000000000000000, -1.000000000000000000, 8.159623473500000156E-13 ) ) ;
#11335 = DIRECTION ( 'NONE',  ( 1.000000000000000000, 2.602084747549999882E-17, 0.000000000000000000 ) ) ;
#11336 = AXIS2_PLACEMENT_3D ( 'NONE', #18794, #2279, #16773 ) ;
#11337 = VERTEX_POINT ( 'NONE', #17421 ) ;
#11338 = VECTOR ( 'NONE', #14648, 1000.000000000000227 ) ;
#11339 = FACE_OUTER_BOUND ( 'NONE', #2480, .T. ) ;
#11340 = LINE ( 'NONE', #4228, #11759 ) ;
#11341 = ORIENTED_EDGE ( 'NONE', *, *, #2533, .F. ) ;
#11342 = CARTESIAN_POINT ( 'NONE',  ( 10.27714235282173938, 13.94660208734305940, -136.0552959530085388 ) ) ;
#11343 = ADVANCED_FACE ( 'NONE', ( #1145 ), #11695, .F. ) ;
#11344 = CARTESIAN_POINT ( 'NONE',  ( 9.182696495386469593, 38.33585586787582855, -141.9420359944410279 ) ) ;
#11345 = EDGE_CURVE ( 'NONE', #5391, #16441, #3041, .T. ) ;
#11346 = VECTOR ( 'NONE', #9652, 1000.000000000000000 ) ;
#11347 = CARTESIAN_POINT ( 'NONE',  ( -5.758148842630000708, -13.22138763369999914, -148.0552959529999839 ) ) ;
#11348 = AXIS2_PLACEMENT_3D ( 'NONE', #11797, #19076, #764 ) ;
#11349 = DIRECTION ( 'NONE',  ( -1.000000000000000000, 0.000000000000000000, 0.000000000000000000 ) ) ;
#11350 = ORIENTED_EDGE ( 'NONE', *, *, #1718, .T. ) ;
#11351 = AXIS2_PLACEMENT_3D ( 'NONE', #4128, #13400, #811 ) ;
#11352 = VECTOR ( 'NONE', #16404, 1000.000000000000114 ) ;
#11353 = AXIS2_PLACEMENT_3D ( 'NONE', #19979, #16630, #5467 ) ;
#11354 = CARTESIAN_POINT ( 'NONE',  ( -34.47299999999999898, 12.24483487620000055, -145.0141470300000037 ) ) ;
#11355 = ORIENTED_EDGE ( 'NONE', *, *, #13026, .F. ) ;
#11356 = ORIENTED_EDGE ( 'NONE', *, *, #21121, .T. ) ;
#11357 = CARTESIAN_POINT ( 'NONE',  ( -26.40742642360234882, 40.79449254541880521, -146.2962172200168993 ) ) ;
#11358 = ORIENTED_EDGE ( 'NONE', *, *, #15208, .T. ) ;
#11359 = CARTESIAN_POINT ( 'NONE',  ( -22.72559961389999827, 32.84666773589999877, -144.4841142160000231 ) ) ;
#11360 = VERTEX_POINT ( 'NONE', #10278 ) ;
#11361 = CARTESIAN_POINT ( 'NONE',  ( 8.250000000000000000, -42.23606797749999942, -150.0552959529999839 ) ) ;
#11362 = B_SPLINE_CURVE_WITH_KNOTS ( 'NONE', 3,
 ( #10818, #1700, #1938, #17989, #16318, #12974, #1813, #3702, #14414, #1587 ),
 .UNSPECIFIED., .F., .F.,
 ( 4, 2, 2, 2, 4 ),
 ( 0.000000000000000000, 0.2500000000000000000, 0.5000000000000000000, 0.7500000000000000000, 1.000000000000000000 ),
 .UNSPECIFIED. ) ;
#11363 = ORIENTED_EDGE ( 'NONE', *, *, #3569, .T. ) ;
#11364 = APPLICATION_PROTOCOL_DEFINITION ( 'draft international standard', 'automotive_design', 1998, #13577 ) ;
#11365 = AXIS2_PLACEMENT_3D ( 'NONE', #6862, #7337, #16149 ) ;
#11366 = ADVANCED_FACE ( 'NONE', ( #6707 ), #17548, .T. ) ;
#11367 = ORIENTED_EDGE ( 'NONE', *, *, #5592, .T. ) ;
#11368 = CARTESIAN_POINT ( 'NONE',  ( -25.35824191590000254, -1.500000000000000000, -145.5657682199999954 ) ) ;
#11369 = CARTESIAN_POINT ( 'NONE',  ( 6.841811532410000396, -13.03968765259999962, -145.5552959529999839 ) ) ;
#11370 = DIRECTION ( 'NONE',  ( 0.000000000000000000, -1.000000000000000000, 2.257144641399999941E-12 ) ) ;
#11371 = CARTESIAN_POINT ( 'NONE',  ( 31.50000000000000000, 40.03620104880000241, -143.0552959529999839 ) ) ;
#11372 = VECTOR ( 'NONE', #1842, 1000.000000000000000 ) ;
#11373 = CONICAL_SURFACE ( 'NONE', #12150, 1.999999999999995115, 0.7853981633970000820 ) ;
#11374 = CARTESIAN_POINT ( 'NONE',  ( -6.171158540472589493, 35.20721382762360463, -148.0504213054279887 ) ) ;
#11375 = VECTOR ( 'NONE', #18436, 1000.000000000000227 ) ;
#11376 = CARTESIAN_POINT ( 'NONE',  ( -8.060394343138106876, 38.95025308942626907, -139.6606609314920604 ) ) ;
#11377 = CIRCLE ( 'NONE', #18254, 10.00000000000000000 ) ;
#11378 = ORIENTED_EDGE ( 'NONE', *, *, #7992, .F. ) ;
#11379 = CARTESIAN_POINT ( 'NONE',  ( -14.47770030809999930, -15.50000000000000000, -147.5552959529999839 ) ) ;
#11380 = CARTESIAN_POINT ( 'NONE',  ( 8.212854026790001427, -28.22404483660000096, -145.0552959529999839 ) ) ;
#11381 = FACE_OUTER_BOUND ( 'NONE', #4842, .T. ) ;
#11382 = ORIENTED_EDGE ( 'NONE', *, *, #12997, .T. ) ;
#11383 = CARTESIAN_POINT ( 'NONE',  ( -11.53909816450000037, 41.50279269539999660, -144.7127947380000137 ) ) ;
#11384 = EDGE_CURVE ( 'NONE', #2111, #16983, #13491, .T. ) ;
#11385 = CARTESIAN_POINT ( 'NONE',  ( -18.53945141080000170, 39.74065879090000664, -147.6687609889999919 ) ) ;
#11386 = CARTESIAN_POINT ( 'NONE',  ( -29.69101630266833425, 40.01133477889813861, -145.8395111173366558 ) ) ;
#11387 = ORIENTED_EDGE ( 'NONE', *, *, #10591, .T. ) ;
#11388 = CARTESIAN_POINT ( 'NONE',  ( -6.323999170589999608, 34.61896835509999448, -147.3311432729999808 ) ) ;
#11389 = CARTESIAN_POINT ( 'NONE',  ( -32.50000000000000000, 51.50000000000000000, -136.0552959530000123 ) ) ;
#11390 = AXIS2_PLACEMENT_3D ( 'NONE', #20554, #11719, #19001 ) ;
#11391 = AXIS2_PLACEMENT_3D ( 'NONE', #814, #7580, #9350 ) ;
#11392 = ORIENTED_EDGE ( 'NONE', *, *, #13153, .F. ) ;
#11393 = CARTESIAN_POINT ( 'NONE',  ( -26.35824191589999899, -1.500000000000000000, -141.0657682190000060 ) ) ;
#11394 = PLANE ( 'NONE',  #1238 ) ;
#11395 = VERTEX_POINT ( 'NONE', #2685 ) ;
#11396 = LINE ( 'NONE', #22359, #10949 ) ;
#11397 = CARTESIAN_POINT ( 'NONE',  ( -20.74418227175951657, 39.28578094477872185, -147.3492911867232067 ) ) ;
#11398 = ORIENTED_EDGE ( 'NONE', *, *, #18752, .T. ) ;
#11399 = CARTESIAN_POINT ( 'NONE',  ( -27.31614846892880166, 35.48399733451186933, -147.3070584612585208 ) ) ;
#11400 = ADVANCED_FACE ( 'NONE', ( #17188 ), #11819, .F. ) ;
#11401 = CARTESIAN_POINT ( 'NONE',  ( -33.42928932190000069, -63.02782287919998794, -141.3604938089999905 ) ) ;
#11402 = ORIENTED_EDGE ( 'NONE', *, *, #16399, .F. ) ;
#11403 = CARTESIAN_POINT ( 'NONE',  ( -13.82058007329999860, 36.03909227049999942, -139.5626078809999910 ) ) ;
#11404 = EDGE_CURVE ( 'NONE', #1427, #13434, #17305, .T. ) ;
#11405 = DIRECTION ( 'NONE',  ( -0.9954742291034677226, 0.09503188512734457583, 4.503363594322118746E-12 ) ) ;
#11406 = CYLINDRICAL_SURFACE ( 'NONE', #18234, 2.000000000000001776 ) ;
#11407 = ADVANCED_FACE ( 'NONE', ( #20038 ), #5054, .T. ) ;
#11408 = ORIENTED_EDGE ( 'NONE', *, *, #22410, .T. ) ;
#11409 = LINE ( 'NONE', #11635, #10576 ) ;
#11410 = ADVANCED_FACE ( 'NONE', ( #1492 ), #9189, .F. ) ;
#11411 = FACE_OUTER_BOUND ( 'NONE', #17742, .T. ) ;
#11412 = EDGE_LOOP ( 'NONE', ( #19885, #370, #7755 ) ) ;
#11413 = VECTOR ( 'NONE', #12606, 1000.000000000000000 ) ;
#11414 = VECTOR ( 'NONE', #88, 1000.000000000000000 ) ;
#11415 = ORIENTED_EDGE ( 'NONE', *, *, #9125, .F. ) ;
#11416 = CARTESIAN_POINT ( 'NONE',  ( -6.774730888589999722, -50.50000000000000000, -149.5552959529999839 ) ) ;
#11417 = DIRECTION ( 'NONE',  ( -1.000000000000000000, 0.000000000000000000, 2.257144641399999941E-12 ) ) ;
#11418 = CARTESIAN_POINT ( 'NONE',  ( 32.14594224149999491, 40.79958733410000349, -136.0552959519999945 ) ) ;
#11419 = FACE_OUTER_BOUND ( 'NONE', #20179, .T. ) ;
#11420 = ORIENTED_EDGE ( 'NONE', *, *, #13176, .F. ) ;
#11421 = FILL_AREA_STYLE ('',( #18703 ) ) ;
#11422 = CARTESIAN_POINT ( 'NONE',  ( -33.50000000000000000, -74.00000000000000000, -132.5552959530000123 ) ) ;
#11423 = EDGE_CURVE ( 'NONE', #20008, #7366, #14447, .T. ) ;
#11424 = DIRECTION ( 'NONE',  ( 0.000000000000000000, 0.000000000000000000, -1.000000000000000000 ) ) ;
#11425 = CARTESIAN_POINT ( 'NONE',  ( 13.09818317349319017, 38.33939095840919720, -136.0552959530295709 ) ) ;
#11426 = CARTESIAN_POINT ( 'NONE',  ( -22.83308877298548012, 39.55027303327759824, -140.7145628016388059 ) ) ;
#11427 = CIRCLE ( 'NONE', #10659, 1.500000000000001332 ) ;
#11428 = AXIS2_PLACEMENT_3D ( 'NONE', #5857, #5743, #3968 ) ;
#11429 = DIRECTION ( 'NONE',  ( 0.000000000000000000, 0.000000000000000000, -1.000000000000000000 ) ) ;
#11430 = EDGE_CURVE ( 'NONE', #4966, #14773, #14568, .T. ) ;
#11431 = CARTESIAN_POINT ( 'NONE',  ( -17.59435718368114721, 36.12650549322601989, -140.0997835545947794 ) ) ;
#11432 = EDGE_CURVE ( 'NONE', #10191, #2371, #16171, .T. ) ;
#11433 = DIRECTION ( 'NONE',  ( 0.000000000000000000, 4.426606872070000353E-37, -1.000000000000000000 ) ) ;
#11434 = DIRECTION ( 'NONE',  ( 2.256861364460000137E-12, 0.000000000000000000, 1.000000000000000000 ) ) ;
#11435 = CARTESIAN_POINT ( 'NONE',  ( 15.50000000000000000, 39.50000000000000000, -151.0552959529999839 ) ) ;
#11436 = ORIENTED_EDGE ( 'NONE', *, *, #5963, .T. ) ;
#11437 = CARTESIAN_POINT ( 'NONE',  ( -5.376163642574164570, 39.00480445835521692, -141.2592359520692753 ) ) ;
#11438 = LINE ( 'NONE', #22170, #8832 ) ;
#11439 = VERTEX_POINT ( 'NONE', #21832 ) ;
#11440 = DIRECTION ( 'NONE',  ( 3.994014902950000436E-29, -1.000000000000000000, 4.148443855749999753E-27 ) ) ;
#11441 = CARTESIAN_POINT ( 'NONE',  ( -22.76238589975820048, 33.93499072747687251, -142.2605165499471696 ) ) ;
#11442 = VECTOR ( 'NONE', #20024, 1000.000000000000000 ) ;
#11443 = DIRECTION ( 'NONE',  ( 1.000000000000000000, 0.000000000000000000, -4.430318231639999944E-12 ) ) ;
#11444 = EDGE_LOOP ( 'NONE', ( #21518, #12485, #850, #20925 ) ) ;
#11445 = VECTOR ( 'NONE', #14534, 1000.000000000000000 ) ;
#11446 = CARTESIAN_POINT ( 'NONE',  ( 22.50000000000000000, 39.50000000000000000, -150.5552959529999839 ) ) ;
#11447 = B_SPLINE_CURVE_WITH_KNOTS ( 'NONE', 3,
 ( #16417, #12830, #17846, #7472, #5223, #7253, #18081, #14273 ),
 .UNSPECIFIED., .F., .F.,
 ( 4, 2, 2, 4 ),
 ( 0.000000000000000000, 0.5000000000000031086, 0.7500000000000015543, 1.000000000000000000 ),
 .UNSPECIFIED. ) ;
#11448 = CARTESIAN_POINT ( 'NONE',  ( 8.212854026790001427, -28.22404483660000096, -145.5552959529999839 ) ) ;
#11449 = DIRECTION ( 'NONE',  ( 0.000000000000000000, 0.000000000000000000, 1.000000000000000000 ) ) ;
#11450 = CARTESIAN_POINT ( 'NONE',  ( -7.500000000000000000, 48.50000000000000000, -151.0552959529999839 ) ) ;
#11451 = DIRECTION ( 'NONE',  ( -2.257157423930000049E-12, 0.000000000000000000, -1.000000000000000000 ) ) ;
#11452 = CARTESIAN_POINT ( 'NONE',  ( 4.301139731426199653, -5.000000000000003553, -136.0552959530097041 ) ) ;
#11453 = VERTEX_POINT ( 'NONE', #12765 ) ;
#11454 = CARTESIAN_POINT ( 'NONE',  ( -28.10506494415270140, 36.10535006841108441, -148.5541524927092780 ) ) ;
#11455 = ADVANCED_FACE ( 'NONE', ( #5516 ), #12651, .T. ) ;
#11456 = ORIENTED_EDGE ( 'NONE', *, *, #16152, .F. ) ;
#11457 = CARTESIAN_POINT ( 'NONE',  ( -14.14505183392335930, 35.98615714182410130, -139.5052020486566562 ) ) ;
#11458 = FACE_OUTER_BOUND ( 'NONE', #5609, .T. ) ;
#11459 = CIRCLE ( 'NONE', #22115, 35.00000000000000000 ) ;
#11460 = AXIS2_PLACEMENT_3D ( 'NONE', #23248, #3369, #17892 ) ;
#11461 = DIRECTION ( 'NONE',  ( -2.602084747549999882E-17, 1.000000000000000000, 5.873289694040000105E-29 ) ) ;
#11462 = AXIS2_PLACEMENT_3D ( 'NONE', #8454, #1101, #19291 ) ;
#11463 = ORIENTED_EDGE ( 'NONE', *, *, #19567, .T. ) ;
#11464 = CARTESIAN_POINT ( 'NONE',  ( -9.999999999969999109, 48.50000000000000000, -137.0552959530000123 ) ) ;
#11465 = CARTESIAN_POINT ( 'NONE',  ( -18.35824191589999899, -34.50000000000000000, -150.0657682190000060 ) ) ;
#11466 = ORIENTED_EDGE ( 'NONE', *, *, #5149, .T. ) ;
#11467 = CARTESIAN_POINT ( 'NONE',  ( -21.11951001670777472, 40.57477398628559939, -141.9750481070400951 ) ) ;
#11468 = CARTESIAN_POINT ( 'NONE',  ( 9.374985222606666113, 38.21845128525978197, -141.8721224038111757 ) ) ;
#11469 = FACE_BOUND ( 'NONE', #2573, .T. ) ;
#11470 = DIRECTION ( 'NONE',  ( 1.000000000000000000, 0.000000000000000000, 2.516505522483685870E-12 ) ) ;
#11471 = DIRECTION ( 'NONE',  ( 2.256967945870000144E-12, 0.000000000000000000, 1.000000000000000000 ) ) ;
#11472 = MECHANICAL_DESIGN_GEOMETRIC_PRESENTATION_REPRESENTATION (  '', ( #9202 ), #17956 ) ;
#11473 = VERTEX_POINT ( 'NONE', #3732 ) ;
#11474 = AXIS2_PLACEMENT_3D ( 'NONE', #12232, #14024, #3092 ) ;
#11475 = DIRECTION ( 'NONE',  ( 4.430318231639999944E-12, -6.100259101500000139E-13, 1.000000000000000000 ) ) ;
#11476 = ORIENTED_EDGE ( 'NONE', *, *, #18776, .F. ) ;
#11477 = DIRECTION ( 'NONE',  ( 1.527666881879999979E-13, 8.171241461240000022E-13, 1.000000000000000000 ) ) ;
#11478 = ORIENTED_EDGE ( 'NONE', *, *, #4894, .F. ) ;
#11479 = ORIENTED_EDGE ( 'NONE', *, *, #21188, .F. ) ;
#11480 = ADVANCED_FACE ( 'NONE', ( #10971 ), #17898, .F. ) ;
#11481 = CARTESIAN_POINT ( 'NONE',  ( -22.60791700490179323, 34.20506515043313556, -140.1155385156617115 ) ) ;
#11482 = EDGE_LOOP ( 'NONE', ( #2365, #9858, #2810 ) ) ;
#11483 = CARTESIAN_POINT ( 'NONE',  ( 1.133692148550000001, -50.50000000000000000, -143.0552959529999839 ) ) ;
#11484 = ADVANCED_FACE ( 'NONE', ( #1965 ), #7180, .T. ) ;
#11485 = VERTEX_POINT ( 'NONE', #14094 ) ;
#11486 = EDGE_LOOP ( 'NONE', ( #14845, #21473, #4996, #20200 ) ) ;
#11487 = DIRECTION ( 'NONE',  ( 2.508215857230000030E-12, 0.000000000000000000, -1.000000000000000000 ) ) ;
#11488 = LINE ( 'NONE', #15197, #19364 ) ;
#11489 = CARTESIAN_POINT ( 'NONE',  ( 12.15117705467117126, 25.45516771066687056, -150.0552959529999839 ) ) ;
#11490 = CARTESIAN_POINT ( 'NONE',  ( -6.033650297970000409, 36.94170754819999303, -147.9652040070000112 ) ) ;
#11491 = FACE_OUTER_BOUND ( 'NONE', #14434, .T. ) ;
#11492 = CARTESIAN_POINT ( 'NONE',  ( -32.50000000000000000, -74.00000000000000000, -132.5552959530000123 ) ) ;
#11493 = EDGE_LOOP ( 'NONE', ( #6918, #11065, #6980, #2703 ) ) ;
#11494 = CARTESIAN_POINT ( 'NONE',  ( -1.550733472792253709, 45.02071668630156154, -150.0552959530000123 ) ) ;
#11495 = CARTESIAN_POINT ( 'NONE',  ( 9.628134746819386081, 36.00655328089813167, -146.3507065506827303 ) ) ;
#11496 = CARTESIAN_POINT ( 'NONE',  ( -13.86630785130000021, -51.50000000000000000, -137.0552959530000123 ) ) ;
#11497 = EDGE_LOOP ( 'NONE', ( #13481, #11775, #5294, #202 ) ) ;
#11498 = CARTESIAN_POINT ( 'NONE',  ( -12.66714788113077894, 37.75265353613255570, -147.6129237411522013 ) ) ;
#11499 = DIRECTION ( 'NONE',  ( 1.000000000000000000, 0.000000000000000000, 0.000000000000000000 ) ) ;
#11500 = PLANE ( 'NONE',  #10988 ) ;
#11501 = EDGE_LOOP ( 'NONE', ( #13929, #15360, #5053, #518, #10290, #9801 ) ) ;
#11502 = FACE_OUTER_BOUND ( 'NONE', #19955, .T. ) ;
#11503 = AXIS2_PLACEMENT_3D ( 'NONE', #1752, #3528, #20060 ) ;
#11504 = CYLINDRICAL_SURFACE ( 'NONE', #5549, 1.500000000000001332 ) ;
#11505 = ORIENTED_EDGE ( 'NONE', *, *, #11113, .T. ) ;
#11506 = CYLINDRICAL_SURFACE ( 'NONE', #7581, 8.176568160360002224 ) ;
#11507 = CARTESIAN_POINT ( 'NONE',  ( -29.03767587600000155, 36.26045984259999955, -140.5446710220000170 ) ) ;
#11508 = ORIENTED_EDGE ( 'NONE', *, *, #8137, .T. ) ;
#11509 = FACE_OUTER_BOUND ( 'NONE', #12108, .T. ) ;
#11510 = CARTESIAN_POINT ( 'NONE',  ( -20.55310894649999653, 37.85259822169999921, -139.7937414779999870 ) ) ;
#11511 = EDGE_CURVE ( 'NONE', #21987, #3746, #17773, .T. ) ;
#11512 = VERTEX_POINT ( 'NONE', #21474 ) ;
#11513 =( LENGTH_UNIT ( ) NAMED_UNIT ( * ) SI_UNIT ( .MILLI., .METRE. ) );
#11514 = CARTESIAN_POINT ( 'NONE',  ( -26.92552552937697996, 36.92880110468703947, -148.2769915172784181 ) ) ;
#11515 = LINE ( 'NONE', #9499, #23200 ) ;
#11516 = VERTEX_POINT ( 'NONE', #12404 ) ;
#11517 = DIRECTION ( 'NONE',  ( -1.000000000000000000, 0.000000000000000000, 0.000000000000000000 ) ) ;
#11518 = PLANE ( 'NONE',  #7288 ) ;
#11519 = CARTESIAN_POINT ( 'NONE',  ( 1.172620240290000115, -63.19354141059999108, -146.5552959529999839 ) ) ;
#11520 = ORIENTED_EDGE ( 'NONE', *, *, #7514, .T. ) ;
#11521 = CARTESIAN_POINT ( 'NONE',  ( -19.59255166829999695, 37.05126161860000167, -140.3061871179999969 ) ) ;
#11522 = EDGE_CURVE ( 'NONE', #22098, #2580, #10852, .T. ) ;
#11523 = DIRECTION ( 'NONE',  ( -2.257171095940000041E-12, 7.494005416210000121E-16, -1.000000000000000000 ) ) ;
#11524 = ORIENTED_EDGE ( 'NONE', *, *, #19945, .T. ) ;
#11525 = ORIENTED_EDGE ( 'NONE', *, *, #22979, .F. ) ;
#11526 = CARTESIAN_POINT ( 'NONE',  ( -34.50000000000000000, 26.00000000000000000, -137.5552959530000123 ) ) ;
#11527 = EDGE_CURVE ( 'NONE', #12071, #9795, #10617, .T. ) ;
#11528 = CARTESIAN_POINT ( 'NONE',  ( -29.94412816097619867, 41.23953273984808021, -145.7122098475038001 ) ) ;
#11529 = PLANE ( 'NONE',  #23468 ) ;
#11530 = DIRECTION ( 'NONE',  ( 5.094701932209999624E-24, 1.000000000000000000, 0.000000000000000000 ) ) ;
#11531 = ORIENTED_EDGE ( 'NONE', *, *, #22917, .F. ) ;
#11532 = CARTESIAN_POINT ( 'NONE',  ( -16.20111387579999729, -34.50000000000000000, -147.8591802640000026 ) ) ;
#11533 = CARTESIAN_POINT ( 'NONE',  ( -8.869124888310000898, 38.72872035620000020, -148.0517159070000162 ) ) ;
#11534 = ADVANCED_FACE ( 'NONE', ( #7064 ), #14323, .F. ) ;
#11535 = CARTESIAN_POINT ( 'NONE',  ( -32.50000000000000000, 48.00000000000000000, -141.5552959529999839 ) ) ;
#11536 = PLANE ( 'NONE',  #12593 ) ;
#11537 = CARTESIAN_POINT ( 'NONE',  ( -24.87949572109999963, 37.83967983510000010, -147.8465544160000036 ) ) ;
#11538 = MANIFOLD_SOLID_BREP ( 'lock_assembly.1\\Part8.1.2\\PartBody', #16777 ) ;
#11539 = CARTESIAN_POINT ( 'NONE',  ( -15.80977837879197878, 32.72809527743532954, -146.2784451626665998 ) ) ;
#11540 = VECTOR ( 'NONE', #20999, 1000.000000000000000 ) ;
#11541 = CARTESIAN_POINT ( 'NONE',  ( -16.99460745035325004, 35.63018681495184126, -140.8504752325732738 ) ) ;
#11542 = CARTESIAN_POINT ( 'NONE',  ( -20.45144833149999997, 36.94873838139999833, -139.8044047869999815 ) ) ;
#11543 = DIRECTION ( 'NONE',  ( -1.000000000000000000, 0.000000000000000000, 0.000000000000000000 ) ) ;
#11544 = DIRECTION ( 'NONE',  ( 0.9949850929136110356, -0.1000233216789610247, 7.446425804567098138E-15 ) ) ;
#11545 = VERTEX_POINT ( 'NONE', #9411 ) ;
#11546 = CARTESIAN_POINT ( 'NONE',  ( -9.335232969524987823, 34.68189297890224765, -146.9285082157170450 ) ) ;
#11547 = CARTESIAN_POINT ( 'NONE',  ( -29.40140556766587920, 40.21055626232655555, -145.9944493861164858 ) ) ;
#11548 = EDGE_CURVE ( 'NONE', #2758, #18780, #22172, .T. ) ;
#11549 = ORIENTED_EDGE ( 'NONE', *, *, #9872, .T. ) ;
#11550 = EDGE_CURVE ( 'NONE', #16851, #20008, #168, .T. ) ;
#11551 = CARTESIAN_POINT ( 'NONE',  ( 1.133692148550000001, 51.00000000000000000, -137.0552959530000123 ) ) ;
#11552 = CARTESIAN_POINT ( 'NONE',  ( -21.23917607303755872, 35.28761490568743397, -147.7082871199631882 ) ) ;
#11553 = FACE_OUTER_BOUND ( 'NONE', #9512, .T. ) ;
#11554 = ORIENTED_EDGE ( 'NONE', *, *, #8235, .T. ) ;
#11555 = CARTESIAN_POINT ( 'NONE',  ( -12.41698512488694028, 36.98746477264878507, -147.4237781434867713 ) ) ;
#11556 = B_SPLINE_CURVE_WITH_KNOTS ( 'NONE', 3,
 ( #12960, #14747, #16884, #2389, #13309, #20578, #13423, #7828, #20462, #16996 ),
 .UNSPECIFIED., .F., .F.,
 ( 4, 2, 2, 2, 4 ),
 ( 0.000000000000000000, 0.2500000000000000000, 0.5000000000000000000, 0.7500000000000000000, 1.000000000000000000 ),
 .UNSPECIFIED. ) ;
#11557 = EDGE_CURVE ( 'NONE', #7409, #4521, #12880, .T. ) ;
#11558 = CARTESIAN_POINT ( 'NONE',  ( -30.49999999990000177, 45.00000000000000000, -140.5552959529999839 ) ) ;
#11559 = EDGE_CURVE ( 'NONE', #11681, #10612, #7756, .T. ) ;
#11560 = CARTESIAN_POINT ( 'NONE',  ( 4.553999924767063057, 13.23986818282688560, -150.0552959530000123 ) ) ;
#11561 = CONTEXT_DEPENDENT_SHAPE_REPRESENTATION ( #16473, #20959 ) ;
#11562 = DIRECTION ( 'NONE',  ( -2.257144641399999941E-12, 0.000000000000000000, -1.000000000000000000 ) ) ;
#11563 = DIRECTION ( 'NONE',  ( 1.000000000000000000, 0.000000000000000000, 0.000000000000000000 ) ) ;
#11564 = EDGE_CURVE ( 'NONE', #12200, #11512, #3853, .T. ) ;
#11565 = CARTESIAN_POINT ( 'NONE',  ( -8.100541861814468447, 36.99062475582145737, -140.7379126119401178 ) ) ;
#11566 = ORIENTED_EDGE ( 'NONE', *, *, #5698, .T. ) ;
#11567 = CARTESIAN_POINT ( 'NONE',  ( -28.21080904470232653, 35.15062816310292959, -148.3093627672952834 ) ) ;
#11568 = ORIENTED_EDGE ( 'NONE', *, *, #4815, .T. ) ;
#11569 = CARTESIAN_POINT ( 'NONE',  ( -13.92432874550000044, 37.01165864720000087, -139.5650670249999905 ) ) ;
#11570 = LINE ( 'NONE', #2556, #5747 ) ;
#11571 = PLANE ( 'NONE',  #4344 ) ;
#11572 = ORIENTED_EDGE ( 'NONE', *, *, #11641, .F. ) ;
#11573 = CARTESIAN_POINT ( 'NONE',  ( 25.49993271309264387, 36.89748944255538987, -136.0552959530575947 ) ) ;
#11574 = DIRECTION ( 'NONE',  ( -0.6459422414661291079, -0.7633862853691523176, -2.245315045000450442E-12 ) ) ;
#11575 = CIRCLE ( 'NONE', #17677, 7.499999999999999112 ) ;
#11576 = ORIENTED_EDGE ( 'NONE', *, *, #12218, .F. ) ;
#11577 = CARTESIAN_POINT ( 'NONE',  ( -20.25327657862008479, 40.16659554823041844, -142.3141480157923411 ) ) ;
#11578 = PRESENTATION_LAYER_ASSIGNMENT (  '', '', ( #209 ) ) ;
#11579 = CARTESIAN_POINT ( 'NONE',  ( -17.42663577349999926, 38.80963643279999786, -139.8270276149999916 ) ) ;
#11580 = CARTESIAN_POINT ( 'NONE',  ( 7.747210282536660664, 35.70138868135349242, -146.1917200021869689 ) ) ;
#11581 = DIRECTION ( 'NONE',  ( 1.000000000000000000, -5.094701932209999624E-24, -2.257144641399999941E-12 ) ) ;
#11582 = EDGE_CURVE ( 'NONE', #11841, #13781, #22285, .T. ) ;
#11583 = CARTESIAN_POINT ( 'NONE',  ( -25.89229443138020414, 34.88584362729995547, -141.2126295570188859 ) ) ;
#11584 = VERTEX_POINT ( 'NONE', #11091 ) ;
#11585 = DIRECTION ( 'NONE',  ( -0.1435602414469281940, -0.9896415801065048257, 3.836930773098079160E-13 ) ) ;
#11586 = EDGE_LOOP ( 'NONE', ( #1702, #7082, #3127, #5653 ) ) ;
#11587 = AXIS2_PLACEMENT_3D ( 'NONE', #8114, #20635, #5984 ) ;
#11588 = DIRECTION ( 'NONE',  ( -0.1577507813030449846, -0.9874789572432817186, 8.298258002992369366E-13 ) ) ;
#11589 = VECTOR ( 'NONE', #13975, 1000.000000000000000 ) ;
#11590 = VERTEX_POINT ( 'NONE', #14795 ) ;
#11591 = CARTESIAN_POINT ( 'NONE',  ( -34.50000000000000000, -18.00000000000000000, -140.0552959529999839 ) ) ;
#11592 = ORIENTED_EDGE ( 'NONE', *, *, #4374, .T. ) ;
#11593 = CARTESIAN_POINT ( 'NONE',  ( -18.00000000000000000, -43.00000000000000000, -140.0552959529999839 ) ) ;
#11594 = VERTEX_POINT ( 'NONE', #18724 ) ;
#11595 = LINE ( 'NONE', #6725, #11013 ) ;
#11596 = VERTEX_POINT ( 'NONE', #16571 ) ;
#11597 = ORIENTED_EDGE ( 'NONE', *, *, #21398, .T. ) ;
#11598 = B_SPLINE_CURVE_WITH_KNOTS ( 'NONE', 3,
 ( #22023, #9619, #11173, #20357, #603, #20589 ),
 .UNSPECIFIED., .F., .F.,
 ( 4, 2, 4 ),
 ( 0.000000000000000000, 0.5000000000000000000, 1.000000000000000000 ),
 .UNSPECIFIED. ) ;
#11599 = CARTESIAN_POINT ( 'NONE',  ( -26.81377270494896337, 41.77330197855063432, -144.5318660586409862 ) ) ;
#11600 = CARTESIAN_POINT ( 'NONE',  ( 16.65835875212643913, -18.90326720743800593, -147.5552959530498640 ) ) ;
#11601 = CARTESIAN_POINT ( 'NONE',  ( -34.50000000000000000, -74.00000000000000000, -155.5552959529999839 ) ) ;
#11602 = CARTESIAN_POINT ( 'NONE',  ( -6.370493725020000220, -17.65251768590000125, -145.5552959529999839 ) ) ;
#11603 = LINE ( 'NONE', #11723, #22071 ) ;
#11604 = CARTESIAN_POINT ( 'NONE',  ( -7.628878236750000319, 37.90286001179999431, -140.0026079769999683 ) ) ;
#11605 = VERTEX_POINT ( 'NONE', #7521 ) ;
#11606 = CARTESIAN_POINT ( 'NONE',  ( 6.500000000000000000, 13.00000000000000000, -150.0552959529999839 ) ) ;
#11607 = VECTOR ( 'NONE', #5699, 1000.000000000000000 ) ;
#11608 = AXIS2_PLACEMENT_3D ( 'NONE', #21219, #12273, #4793 ) ;
#11609 = EDGE_CURVE ( 'NONE', #15560, #22352, #1209, .T. ) ;
#11610 = EDGE_CURVE ( 'NONE', #5331, #7124, #11315, .T. ) ;
#11611 = CARTESIAN_POINT ( 'NONE',  ( 9.918657622369268623, 37.48996405937540999, -146.5072937552601218 ) ) ;
#11612 = CARTESIAN_POINT ( 'NONE',  ( 24.90191174485078207, 38.33948587671270047, -150.0552959529999839 ) ) ;
#11613 = ADVANCED_FACE ( 'NONE', ( #22059 ), #15139, .F. ) ;
#11614 = VERTEX_POINT ( 'NONE', #20504 ) ;
#11615 = CARTESIAN_POINT ( 'NONE',  ( 15.87827223000000032, -26.60524292859999917, -144.5552959529999839 ) ) ;
#11616 = CARTESIAN_POINT ( 'NONE',  ( 4.750000000030000002, -40.36803398869999882, -136.0552959530000123 ) ) ;
#11617 = EDGE_LOOP ( 'NONE', ( #13152, #23102, #6682, #1539 ) ) ;
#11618 = DIRECTION ( 'NONE',  ( 0.000000000000000000, -1.000000000000000000, 8.159623473500000156E-13 ) ) ;
#11619 =( BOUNDED_SURFACE ( )  B_SPLINE_SURFACE ( 5, 5, ( 
 ( #562, #21979, #2356, #11021, #18299, #16852 ),
 ( #18176, #9336, #5669, #20080, #12805, #9114 ),
 ( #3900, #2012, #7795, #5558, #9233, #3661 ),
 ( #15063, #12925, #5448, #16499, #206, #12693 ),
 ( #1891, #16610, #11130, #3779, #7450, #16395 ),
 ( #18406, #2115, #14712, #321, #7682, #19960 ),
 ( #5899, #7564, #2232, #4010, #10897, #7346 ),
 ( #14840, #11357, #5786, #13045, #9452, #20314 ),
 ( #11239, #18511, #16730, #445, #14951, #13155 ),
 ( #18639, #20424, #4118, #6017, #15188, #16964 ),
 ( #22443, #15414, #13505, #675, #22673, #9689 ),
 ( #801, #6368, #19106, #10039, #10163, #18757 ) ),
 .UNSPECIFIED., .F., .F., .F. ) 
 B_SPLINE_SURFACE_WITH_KNOTS ( ( 6, 3, 3, 6 ),
 ( 6, 6 ),
 ( 0.000000000000000000, 4.469553974960000176, 8.969854531369998440, 13.50363095830000049 ),
 ( 1.570796326695754974, 3.141592653590000062 ),
 .UNSPECIFIED. ) 
 GEOMETRIC_REPRESENTATION_ITEM ( )  RATIONAL_B_SPLINE_SURFACE ( (
 ( 0.2500000000000000000, 0.2499999999873634970, 0.2999999999810455398, 0.3999999999747270163, 0.5999999999747269719, 1.000000000000000000),
 ( 0.2500000000000000000, 0.2499999999873634970, 0.2999999999810455398, 0.3999999999747270163, 0.5999999999747269719, 1.000000000000000000),
 ( 0.2500000000000000000, 0.2499999999873634970, 0.2999999999810455398, 0.3999999999747270163, 0.5999999999747269719, 1.000000000000000000),
 ( 0.2500000000000000000, 0.2499999999873634970, 0.2999999999810455398, 0.3999999999747270163, 0.5999999999747269719, 1.000000000000000000),
 ( 0.2500000000000000000, 0.2499999999873634970, 0.2999999999810455398, 0.3999999999747270163, 0.5999999999747269719, 1.000000000000000000),
 ( 0.2500000000000000000, 0.2499999999873634970, 0.2999999999810455398, 0.3999999999747270163, 0.5999999999747269719, 1.000000000000000000),
 ( 0.2500000000000000000, 0.2499999999873634970, 0.2999999999810455398, 0.3999999999747270163, 0.5999999999747269719, 1.000000000000000000),
 ( 0.2500000000000000000, 0.2499999999873634970, 0.2999999999810455398, 0.3999999999747270163, 0.5999999999747269719, 1.000000000000000000),
 ( 0.2500000000000000000, 0.2499999999873634970, 0.2999999999810455398, 0.3999999999747270163, 0.5999999999747269719, 1.000000000000000000),
 ( 0.2500000000000000000, 0.2499999999873634970, 0.2999999999810455398, 0.3999999999747270163, 0.5999999999747269719, 1.000000000000000000),
 ( 0.2500000000000000000, 0.2499999999873634970, 0.2999999999810455398, 0.3999999999747270163, 0.5999999999747269719, 1.000000000000000000),
 ( 0.2500000000000000000, 0.2499999999873634970, 0.2999999999810455398, 0.3999999999747270163, 0.5999999999747269719, 1.000000000000000000) ) ) 
 REPRESENTATION_ITEM ( '' )  SURFACE ( )  );
#11620 = ORIENTED_EDGE ( 'NONE', *, *, #5268, .F. ) ;
#11621 = DIRECTION ( 'NONE',  ( 0.7633862853691523176, 0.6459422414661291079, 0.000000000000000000 ) ) ;
#11622 = CARTESIAN_POINT ( 'NONE',  ( 22.50000000000000000, 36.50000000000000000, -136.0552959530000123 ) ) ;
#11623 = ORIENTED_EDGE ( 'NONE', *, *, #22849, .T. ) ;
#11624 = CARTESIAN_POINT ( 'NONE',  ( -13.92432874550000044, 37.01165864720000087, -139.5650670249999905 ) ) ;
#11625 = CIRCLE ( 'NONE', #10097, 2.000000000000000000 ) ;
#11626 = VERTEX_POINT ( 'NONE', #9540 ) ;
#11627 = CARTESIAN_POINT ( 'NONE',  ( -29.03767587600000155, 36.26045984259999955, -140.5446710220000170 ) ) ;
#11628 = CYLINDRICAL_SURFACE ( 'NONE', #19539, 7.500000000000007105 ) ;
#11629 = ORIENTED_EDGE ( 'NONE', *, *, #7620, .F. ) ;
#11630 = LINE ( 'NONE', #14879, #14027 ) ;
#11631 = DIRECTION ( 'NONE',  ( -1.457881434619999915E-12, -1.723066134219999902E-12, 1.000000000000000000 ) ) ;
#11632 = ORIENTED_EDGE ( 'NONE', *, *, #12296, .T. ) ;
#11633 = CARTESIAN_POINT ( 'NONE',  ( -11.10890527109999937, 34.84141842859999372, -140.9538660569999990 ) ) ;
#11634 = VERTEX_POINT ( 'NONE', #18475 ) ;
#11635 = CARTESIAN_POINT ( 'NONE',  ( 1.133692148650000009, -2.273736754430000208E-12, -136.0552959530000123 ) ) ;
#11636 = DIRECTION ( 'NONE',  ( -0.1000233216789610108, -0.9949850929136109245, 3.559993607998610461E-13 ) ) ;
#11637 = ORIENTED_EDGE ( 'NONE', *, *, #6179, .F. ) ;
#11638 = VECTOR ( 'NONE', #15277, 1000.000000000000000 ) ;
#11639 = ADVANCED_FACE ( 'NONE', ( #2188 ), #405, .T. ) ;
#11640 = AXIS2_PLACEMENT_3D ( 'NONE', #4941, #8497, #1502 ) ;
#11641 = EDGE_CURVE ( 'NONE', #5292, #3235, #4206, .T. ) ;
#11642 = ORIENTED_EDGE ( 'NONE', *, *, #15099, .F. ) ;
#11643 = CARTESIAN_POINT ( 'NONE',  ( 1.578081969995051459, -2.714756346922164720, -150.0552959530000123 ) ) ;
#11644 = CARTESIAN_POINT ( 'NONE',  ( -30.35298369712678124, 40.05084304751723323, -145.7710807886656994 ) ) ;
#11645 = CARTESIAN_POINT ( 'NONE',  ( -13.36469768600054131, 37.07845968427642447, -139.9331372610152187 ) ) ;
#11646 = CARTESIAN_POINT ( 'NONE',  ( -32.50000000000000000, -51.50000000000000000, -136.0552959519999945 ) ) ;
#11647 = VERTEX_POINT ( 'NONE', #20853 ) ;
#11648 = DIRECTION ( 'NONE',  ( 2.259525899719999991E-12, 0.000000000000000000, -1.000000000000000000 ) ) ;
#11649 = FACE_OUTER_BOUND ( 'NONE', #11486, .T. ) ;
#11650 = DIRECTION ( 'NONE',  ( 0.4794255386042040601, 0.8775825618903723147, 0.000000000000000000 ) ) ;
#11651 = CARTESIAN_POINT ( 'NONE',  ( 18.95053822279999878, -51.50000000000000000, -150.0552959529999839 ) ) ;
#11652 = CARTESIAN_POINT ( 'NONE',  ( -24.01715389780000010, 40.57582142210000598, -141.9832779239999923 ) ) ;
#11653 = CARTESIAN_POINT ( 'NONE',  ( -16.35051094559660001, 37.08015310165674805, -139.9332297721434770 ) ) ;
#11654 = VECTOR ( 'NONE', #262, 1000.000000000000000 ) ;
#11655 = FACE_OUTER_BOUND ( 'NONE', #21380, .T. ) ;
#11656 = VECTOR ( 'NONE', #6085, 1000.000000000000000 ) ;
#11657 = DIRECTION ( 'NONE',  ( 0.000000000000000000, 1.000000000000000000, 0.000000000000000000 ) ) ;
#11658 = CARTESIAN_POINT ( 'NONE',  ( -32.50000000000000000, -50.00000000000000000, -149.5552959529999839 ) ) ;
#11659 = CARTESIAN_POINT ( 'NONE',  ( -1.500000000000000000, 44.50000000000000000, -150.5552959529999839 ) ) ;
#11660 = ADVANCED_FACE ( 'NONE', ( #4428 ), #17159, .F. ) ;
#11661 = VERTEX_POINT ( 'NONE', #15378 ) ;
#11662 = CARTESIAN_POINT ( 'NONE',  ( -10.66194399686184013, 33.15920395727439995, -144.2988335297578146 ) ) ;
#11663 = LINE ( 'NONE', #4203, #2776 ) ;
#11664 = CARTESIAN_POINT ( 'NONE',  ( 22.42370904790000097, -21.41421288319999761, -143.0552959529999839 ) ) ;
#11665 = VERTEX_POINT ( 'NONE', #3010 ) ;
#11666 = DIRECTION ( 'NONE',  ( 1.000000000000000000, 0.000000000000000000, 0.000000000000000000 ) ) ;
#11667 = CARTESIAN_POINT ( 'NONE',  ( -22.34741274029249425, 33.98766409949738687, -142.2380615103167543 ) ) ;
#11668 = EDGE_CURVE ( 'NONE', #13199, #4045, #22635, .T. ) ;
#11669 = CARTESIAN_POINT ( 'NONE',  ( -8.734077015120000453, -11.22642389220000148, -145.5552959529999839 ) ) ;
#11670 = EDGE_LOOP ( 'NONE', ( #9283, #20603 ) ) ;
#11671 = CARTESIAN_POINT ( 'NONE',  ( -22.78427419138386867, 39.31013640214133176, -141.0476221778322667 ) ) ;
#11672 = AXIS2_PLACEMENT_3D ( 'NONE', #21845, #19930, #1628 ) ;
#11673 = CARTESIAN_POINT ( 'NONE',  ( 8.500000000050000892, 37.00000000000000000, -148.7552959530000010 ) ) ;
#11674 = AXIS2_PLACEMENT_3D ( 'NONE', #8549, #2986, #22727 ) ;
#11675 = CARTESIAN_POINT ( 'NONE',  ( 2.170391987449999505, -12.72823260819999902, -146.0552959529999839 ) ) ;
#11676 = DIRECTION ( 'NONE',  ( -5.094701932209999624E-24, -1.000000000000000000, 1.149947916579999802E-35 ) ) ;
#11677 = CARTESIAN_POINT ( 'NONE',  ( 0.8371776177479999248, 14.00000000000000000, -144.0552959529999839 ) ) ;
#11678 = CARTESIAN_POINT ( 'NONE',  ( -32.50000000000000000, 28.00000000000000000, -141.5552959529999839 ) ) ;
#11679 = CARTESIAN_POINT ( 'NONE',  ( -8.150249107171578800, 40.14823067250430455, -142.2562647667796512 ) ) ;
#11680 = EDGE_CURVE ( 'NONE', #8910, #20128, #6449, .T. ) ;
#11681 = VERTEX_POINT ( 'NONE', #19066 ) ;
#11682 = CARTESIAN_POINT ( 'NONE',  ( -28.54685876571991798, 33.62064205115557058, -146.0221638278284786 ) ) ;
#11683 = VERTEX_POINT ( 'NONE', #11913 ) ;
#11684 = CARTESIAN_POINT ( 'NONE',  ( -13.69140658673902600, 32.73813017274896708, -141.7795096389974105 ) ) ;
#11685 = DIRECTION ( 'NONE',  ( -0.9980143568310856361, 0.06298685227120542907, 4.509810669690391193E-12 ) ) ;
#11686 = FACE_OUTER_BOUND ( 'NONE', #11670, .T. ) ;
#11687 = AXIS2_PLACEMENT_3D ( 'NONE', #7974, #22510, #11650 ) ;
#11688 = EDGE_CURVE ( 'NONE', #13163, #11906, #15491, .T. ) ;
#11689 = ORIENTED_EDGE ( 'NONE', *, *, #14197, .F. ) ;
#11690 = DIRECTION ( 'NONE',  ( 0.000000000000000000, -1.100009706970682018E-14, -1.000000000000000000 ) ) ;
#11691 = DIRECTION ( 'NONE',  ( 1.000000000000000000, 0.000000000000000000, 0.000000000000000000 ) ) ;
#11692 = EDGE_CURVE ( 'NONE', #11694, #10188, #4550, .T. ) ;
#11693 = MANIFOLD_SOLID_BREP ( 'Stock-MAS-159-1', #13340 ) ;
#11694 = VERTEX_POINT ( 'NONE', #11790 ) ;
#11695 = CYLINDRICAL_SURFACE ( 'NONE', #11784, 0.7500000000000006661 ) ;
#11696 = ADVANCED_FACE ( 'NONE', ( #10003 ), #17514, .T. ) ;
#11697 = EDGE_CURVE ( 'NONE', #20106, #6084, #22852, .T. ) ;
#11698 = CARTESIAN_POINT ( 'NONE',  ( -18.17958360501333459, 40.51113216957658381, -141.8712026623171312 ) ) ;
#11699 = CARTESIAN_POINT ( 'NONE',  ( 7.039467463307463646, 37.39727521495605345, -146.5309852632870786 ) ) ;
#11700 = DIRECTION ( 'NONE',  ( 2.257749542879999954E-12, 0.000000000000000000, 1.000000000000000000 ) ) ;
#11701 = CARTESIAN_POINT ( 'NONE',  ( -25.17490547269999723, 35.46855981759999565, -147.6699473629999773 ) ) ;
#11702 = FACE_OUTER_BOUND ( 'NONE', #11953, .T. ) ;
#11703 = CIRCLE ( 'NONE', #23129, 2.000000000000000000 ) ;
#11704 = VECTOR ( 'NONE', #12254, 1000.000000000000000 ) ;
#11705 = ORIENTED_EDGE ( 'NONE', *, *, #10681, .F. ) ;
#11706 = CARTESIAN_POINT ( 'NONE',  ( 9.183200060760000838, 0.4999999999990000776, -148.5552959529999839 ) ) ;
#11707 = EDGE_CURVE ( 'NONE', #11140, #2330, #20550, .T. ) ;
#11708 = CIRCLE ( 'NONE', #10574, 1.500000000000000444 ) ;
#11709 = ORIENTED_EDGE ( 'NONE', *, *, #16396, .F. ) ;
#11710 = FILL_AREA_STYLE_COLOUR ( '', #8430 ) ;
#11711 = ORIENTED_EDGE ( 'NONE', *, *, #23303, .F. ) ;
#11712 = VECTOR ( 'NONE', #5245, 1000.000000000000000 ) ;
#11713 = DIRECTION ( 'NONE',  ( 1.000000000000000000, 0.000000000000000000, -2.257453483404484831E-12 ) ) ;
#11714 = VERTEX_POINT ( 'NONE', #15617 ) ;
#11715 = CARTESIAN_POINT ( 'NONE',  ( -0.9999999999639999082, 20.50000000000000000, -136.0552959530000123 ) ) ;
#11716 = ORIENTED_EDGE ( 'NONE', *, *, #12811, .F. ) ;
#11717 = ORIENTED_EDGE ( 'NONE', *, *, #10102, .F. ) ;
#11718 = CARTESIAN_POINT ( 'NONE',  ( 0.5000000001500000124, 16.89444872450000190, -143.5552959529999839 ) ) ;
#11719 = DIRECTION ( 'NONE',  ( -2.507771768022264771E-12, -1.592655090489709912E-17, 1.000000000000000000 ) ) ;
#11720 = ADVANCED_FACE ( 'NONE', ( #22881 ), #21038, .F. ) ;
#11721 = CARTESIAN_POINT ( 'NONE',  ( -11.15746551791342256, 40.20079968431886641, -142.3617349190212451 ) ) ;
#11722 = CARTESIAN_POINT ( 'NONE',  ( -11.99109128271716607, 36.93662743998936548, -148.3295785880283688 ) ) ;
#11723 = CARTESIAN_POINT ( 'NONE',  ( -13.86630785140000022, -51.00000000000000000, -137.0552959530000123 ) ) ;
#11724 = CARTESIAN_POINT ( 'NONE',  ( -8.672768080054304107, 41.10012672573470383, -146.4297548272103882 ) ) ;
#11725 = ORIENTED_EDGE ( 'NONE', *, *, #5620, .T. ) ;
#11726 = AXIS2_PLACEMENT_3D ( 'NONE', #19546, #14422, #10474 ) ;
#11727 = CARTESIAN_POINT ( 'NONE',  ( -12.50000000000000000, 42.50000000000000000, -137.0552959530000123 ) ) ;
#11728 = CARTESIAN_POINT ( 'NONE',  ( 9.795489902830604834, 36.24188551843280237, -146.4379907056267882 ) ) ;
#11729 = AXIS2_PLACEMENT_3D ( 'NONE', #10528, #15902, #3073 ) ;
#11730 = CARTESIAN_POINT ( 'NONE',  ( 4.999999999879999990, -4.750000000000000000, -135.0552959530000123 ) ) ;
#11731 = ORIENTED_EDGE ( 'NONE', *, *, #16454, .F. ) ;
#11732 = CARTESIAN_POINT ( 'NONE',  ( -17.98964812796958057, 38.50830570030355915, -147.4920370692187817 ) ) ;
#11733 = CARTESIAN_POINT ( 'NONE',  ( -25.85824191589999899, -34.50000000000000000, -144.8157682190000060 ) ) ;
#11734 = ORIENTED_EDGE ( 'NONE', *, *, #3938, .F. ) ;
#11735 = CARTESIAN_POINT ( 'NONE',  ( -30.35298369712675637, 40.05084304751726165, -145.7710807886656141 ) ) ;
#11736 = VECTOR ( 'NONE', #19070, 1000.000000000000000 ) ;
#11737 = ORIENTED_EDGE ( 'NONE', *, *, #2419, .T. ) ;
#11738 = CARTESIAN_POINT ( 'NONE',  ( 8.750000000030000891, -42.36803398869999882, -137.0552959530000123 ) ) ;
#11739 = DIRECTION ( 'NONE',  ( -1.527666881879999979E-13, -8.171241461240000022E-13, -1.000000000000000000 ) ) ;
#11740 = ORIENTED_EDGE ( 'NONE', *, *, #4594, .F. ) ;
#11741 = CARTESIAN_POINT ( 'NONE',  ( -15.14642988953127123, 40.61711729829275441, -143.6018754827553039 ) ) ;
#11742 = AXIS2_PLACEMENT_3D ( 'NONE', #20142, #6083, #9167 ) ;
#11743 = CARTESIAN_POINT ( 'NONE',  ( -26.12537298186485302, 35.02184044444919664, -139.7119552129821898 ) ) ;
#11744 = VERTEX_POINT ( 'NONE', #10269 ) ;
#11745 = AXIS2_PLACEMENT_3D ( 'NONE', #7326, #17797, #9091 ) ;
#11746 = CARTESIAN_POINT ( 'NONE',  ( 22.50000000000000000, 39.50000000000000000, -136.0552959530000123 ) ) ;
#11747 = ADVANCED_FACE ( 'NONE', ( #19315 ), #4688, .F. ) ;
#11748 = VERTEX_POINT ( 'NONE', #11805 ) ;
#11749 = AXIS2_PLACEMENT_3D ( 'NONE', #11050, #18328, #2040 ) ;
#11750 = CYLINDRICAL_SURFACE ( 'NONE', #3793, 2.000000000000002220 ) ;
#11751 = DIRECTION ( 'NONE',  ( -1.000000000000000000, 1.190078432789999897E-50, 2.257144641399999941E-12 ) ) ;
#11752 = EDGE_LOOP ( 'NONE', ( #19633, #12812, #13940, #13486 ) ) ;
#11753 = LINE ( 'NONE', #9971, #16349 ) ;
#11754 = EDGE_LOOP ( 'NONE', ( #5343, #14948, #4433, #3261 ) ) ;
#11755 = DIRECTION ( 'NONE',  ( 0.000000000000000000, 1.000000000000000000, 0.000000000000000000 ) ) ;
#11756 = CARTESIAN_POINT ( 'NONE',  ( 12.50000000010000001, 16.89444872450000190, -143.5552959529999839 ) ) ;
#11757 = EDGE_LOOP ( 'NONE', ( #18405, #19142, #7278, #9821 ) ) ;
#11758 = VERTEX_POINT ( 'NONE', #10484 ) ;
#11759 = VECTOR ( 'NONE', #9436, 1000.000000000000000 ) ;
#11760 =( BOUNDED_CURVE ( )  B_SPLINE_CURVE ( 5, ( #8876, #1655, #14366, #5326, #12690, #7105 ),
 .UNSPECIFIED., .F., .F. ) 
 B_SPLINE_CURVE_WITH_KNOTS ( ( 6, 6 ),
 ( 1.570796326683616906, 3.141592653590000062 ),
 .UNSPECIFIED. ) 
 CURVE ( )  GEOMETRIC_REPRESENTATION_ITEM ( )  RATIONAL_B_SPLINE_CURVE ( ( 0.2499999999999999722, 0.2499999999858182609, 0.2999999999787273941, 0.3999999999716365440, 0.5999999999716365551, 1.000000000000000000 ) ) 
 REPRESENTATION_ITEM ( '' )  );
#11761 = VECTOR ( 'NONE', #18851, 1000.000000000000000 ) ;
#11762 = PLANE ( 'NONE',  #2906 ) ;
#11763 = CARTESIAN_POINT ( 'NONE',  ( -21.21916986627255852, 36.96385231547830585, -148.6710958206780333 ) ) ;
#11764 = AXIS2_PLACEMENT_3D ( 'NONE', #13764, #3061, #17917 ) ;
#11765 = DIRECTION ( 'NONE',  ( -1.211690350419999855E-27, -2.765629237170000203E-27, 1.000000000000000000 ) ) ;
#11766 = DIRECTION ( 'NONE',  ( -1.000000000000000000, 0.000000000000000000, 2.257120985840000117E-12 ) ) ;
#11767 = ORIENTED_EDGE ( 'NONE', *, *, #741, .T. ) ;
#11768 = CARTESIAN_POINT ( 'NONE',  ( -30.49999999990000177, 47.50000000000000000, -139.0552959529999839 ) ) ;
#11769 = CARTESIAN_POINT ( 'NONE',  ( 1.847645635000000119, -15.93876195360000025, -146.0552959529999839 ) ) ;
#11770 = B_SPLINE_CURVE_WITH_KNOTS ( 'NONE', 3,
 ( #20083, #14257, #23536, #19854, #16163, #3551, #15918, #3310, #3782, #17708 ),
 .UNSPECIFIED., .F., .F.,
 ( 4, 2, 2, 2, 4 ),
 ( 0.000000000000000000, 0.2500000000000000000, 0.5000000000000000000, 0.7500000000000000000, 1.000000000000000000 ),
 .UNSPECIFIED. ) ;
#11771 = DIRECTION ( 'NONE',  ( 1.000000000000000000, 0.000000000000000000, 0.000000000000000000 ) ) ;
#11772 = FACE_OUTER_BOUND ( 'NONE', #1526, .T. ) ;
#11773 = CARTESIAN_POINT ( 'NONE',  ( 19.68320006079999729, -16.50000000000000000, -150.0552959529999839 ) ) ;
#11774 = MANIFOLD_SOLID_BREP ( 'lock_assembly.1\\lock body.1\\PartBody', #442 ) ;
#11775 = ORIENTED_EDGE ( 'NONE', *, *, #363, .T. ) ;
#11776 = CARTESIAN_POINT ( 'NONE',  ( -16.82851227082468171, 36.09362984996642609, -139.4602078708371948 ) ) ;
#11777 = EDGE_CURVE ( 'NONE', #12052, #19107, #11928, .T. ) ;
#11778 = CARTESIAN_POINT ( 'NONE',  ( -15.90559286389999905, 34.15404988380000617, -147.7469703310000000 ) ) ;
#11779 = CARTESIAN_POINT ( 'NONE',  ( -5.647208160064898230, 36.92537127315613787, -140.1716802709670731 ) ) ;
#11780 = DIRECTION ( 'NONE',  ( 1.000000000000000000, 0.000000000000000000, -1.480297366166875808E-13 ) ) ;
#11781 = EDGE_CURVE ( 'NONE', #3115, #10871, #23123, .T. ) ;
#11782 = CARTESIAN_POINT ( 'NONE',  ( -13.86630785140000022, -50.50000000000000000, -137.0552959530000123 ) ) ;
#11783 = AXIS2_PLACEMENT_3D ( 'NONE', #7017, #10692, #21548 ) ;
#11784 = AXIS2_PLACEMENT_3D ( 'NONE', #15403, #4814, #15646 ) ;
#11785 = EDGE_LOOP ( 'NONE', ( #9162, #23360, #9867, #4569 ) ) ;
#11786 = DIRECTION ( 'NONE',  ( 1.527666881879999979E-13, 8.153477892850000134E-13, 1.000000000000000000 ) ) ;
#11787 = CARTESIAN_POINT ( 'NONE',  ( -24.00000000000000000, 21.50000000000000000, -151.0552959529999839 ) ) ;
#11788 = CARTESIAN_POINT ( 'NONE',  ( -32.50000000000000000, -51.50000000000000000, -137.0552959530000123 ) ) ;
#11789 = ORIENTED_EDGE ( 'NONE', *, *, #17554, .F. ) ;
#11790 = CARTESIAN_POINT ( 'NONE',  ( 2.500000000130000011, 16.50000000000000000, -150.5552959529999839 ) ) ;
#11791 = CARTESIAN_POINT ( 'NONE',  ( -28.14969746246292104, 32.41805236246676003, -143.4814202872532007 ) ) ;
#11792 = CARTESIAN_POINT ( 'NONE',  ( -31.00000000000000000, 1.000000000000000000, -149.5552959529999839 ) ) ;
#11793 = ORIENTED_EDGE ( 'NONE', *, *, #12838, .F. ) ;
#11794 = CARTESIAN_POINT ( 'NONE',  ( -13.36469768600054131, 37.07845968427642447, -139.9331372610152187 ) ) ;
#11795 = CARTESIAN_POINT ( 'NONE',  ( -17.22605506639999717, 36.97564272059999979, -139.5994799229999899 ) ) ;
#11796 = CARTESIAN_POINT ( 'NONE',  ( -32.50000000000000000, -43.00000000050000182, -137.0552959530000123 ) ) ;
#11797 = CARTESIAN_POINT ( 'NONE',  ( -31.00000000000000000, -50.00000000000000000, -149.5552959529999839 ) ) ;
#11798 = AXIS2_PLACEMENT_3D ( 'NONE', #18160, #3531, #7213 ) ;
#11799 = CARTESIAN_POINT ( 'NONE',  ( -9.429756658493721133, 34.97621497276782065, -148.2829651374544540 ) ) ;
#11800 = AXIS2_PLACEMENT_3D ( 'NONE', #7341, #5893, #18170 ) ;
#11801 = LINE ( 'NONE', #7766, #16924 ) ;
#11802 = STYLED_ITEM ( 'NONE', ( #5043 ), #11774 ) ;
#11803 = CARTESIAN_POINT ( 'NONE',  ( 6.446555752716397691, -33.00005219093733899, -150.0552959529999555 ) ) ;
#11804 = ORIENTED_EDGE ( 'NONE', *, *, #22047, .F. ) ;
#11805 = CARTESIAN_POINT ( 'NONE',  ( 19.13369214879999802, -50.49999999980000354, -149.5552959529999839 ) ) ;
#11806 = ORIENTED_EDGE ( 'NONE', *, *, #10611, .T. ) ;
#11807 = PRODUCT_DEFINITION_SHAPE ( 'NONE', 'NONE',  #23548 ) ;
#11808 = CARTESIAN_POINT ( 'NONE',  ( -13.64404366343704034, 33.71937897323879696, -142.3027892630092026 ) ) ;
#11809 = CARTESIAN_POINT ( 'NONE',  ( -22.52780672249999938, 37.05898997719999954, -140.0074087190000114 ) ) ;
#11810 = EDGE_CURVE ( 'NONE', #5668, #12787, #13722, .T. ) ;
#11811 = DIRECTION ( 'NONE',  ( 1.211690350419999855E-27, 2.765629237170000203E-27, -1.000000000000000000 ) ) ;
#11812 = ORIENTED_EDGE ( 'NONE', *, *, #2645, .T. ) ;
#11813 = PLANE ( 'NONE',  #8727 ) ;
#11814 = CARTESIAN_POINT ( 'NONE',  ( -13.92432874550000044, 37.01165864720000087, -139.5650670249999905 ) ) ;
#11815 = MANIFOLD_SOLID_BREP ( 'lock_assembly.1\\deadbolt_assembly\\Product2.1\\dead bolt perpendicular.1\\PartBody', #17545 ) ;
#11816 = AXIS2_PLACEMENT_3D ( 'NONE', #18863, #8697, #7047 ) ;
#11817 = ORIENTED_EDGE ( 'NONE', *, *, #2979, .F. ) ;
#11818 = VECTOR ( 'NONE', #15012, 1000.000000000000000 ) ;
#11819 = PLANE ( 'NONE',  #2690 ) ;
#11820 = EDGE_CURVE ( 'NONE', #14446, #19224, #6814, .T. ) ;
#11821 = CARTESIAN_POINT ( 'NONE',  ( -16.91592704275090142, 37.75347730504772414, -140.5160138912785897 ) ) ;
#11822 = CARTESIAN_POINT ( 'NONE',  ( 7.894323098160722196, 35.62746767956905813, -146.1448649138240512 ) ) ;
#11823 = DIRECTION ( 'NONE',  ( 1.211690350419999855E-27, 2.765629237170000203E-27, -1.000000000000000000 ) ) ;
#11824 = CARTESIAN_POINT ( 'NONE',  ( -25.36170170592352235, 36.30663503025585470, -140.4342969991932364 ) ) ;
#11825 = CYLINDRICAL_SURFACE ( 'NONE', #2181, 4.999999999999998224 ) ;
#11826 = ADVANCED_FACE ( 'NONE', ( #23361 ), #5392, .T. ) ;
#11827 = ADVANCED_FACE ( 'NONE', ( #3365 ), #6938, .T. ) ;
#11828 = ORIENTED_EDGE ( 'NONE', *, *, #15787, .F. ) ;
#11829 = DIRECTION ( 'NONE',  ( -2.256894259919999967E-12, 0.000000000000000000, 1.000000000000000000 ) ) ;
#11830 = AXIS2_PLACEMENT_3D ( 'NONE', #21406, #15802, #19500 ) ;
#11831 = VECTOR ( 'NONE', #396, 1000.000000000000000 ) ;
#11832 = VECTOR ( 'NONE', #8561, 1000.000000000000114 ) ;
#11833 = EDGE_CURVE ( 'NONE', #4825, #20191, #19079, .T. ) ;
#11834 = ORIENTED_EDGE ( 'NONE', *, *, #16090, .F. ) ;
#11835 = ORIENTED_EDGE ( 'NONE', *, *, #5736, .F. ) ;
#11836 = DIRECTION ( 'NONE',  ( -1.000000000000000000, 1.190078432789999897E-50, 2.257144641399999941E-12 ) ) ;
#11837 = EDGE_CURVE ( 'NONE', #16366, #18905, #9177, .T. ) ;
#11838 = ORIENTED_EDGE ( 'NONE', *, *, #23033, .F. ) ;
#11839 = CARTESIAN_POINT ( 'NONE',  ( 6.500000000040000003, 28.00000000000000000, -136.0552959530000123 ) ) ;
#11840 = ORIENTED_EDGE ( 'NONE', *, *, #16494, .T. ) ;
#11841 = VERTEX_POINT ( 'NONE', #19910 ) ;
#11842 = DIRECTION ( 'NONE',  ( 0.000000000000000000, -1.000000000000000000, 8.159623473500000156E-13 ) ) ;
#11843 = CARTESIAN_POINT ( 'NONE',  ( -18.28451977759775815, 36.23520409079904425, -147.6763998120985946 ) ) ;
#11844 = CARTESIAN_POINT ( 'NONE',  ( -10.69115198329542160, 37.03949207291182688, -140.6562969416297335 ) ) ;
#11845 = CYLINDRICAL_SURFACE ( 'NONE', #23130, 1.499999999999999556 ) ;
#11846 = LINE ( 'NONE', #15783, #2326 ) ;
#11847 = CARTESIAN_POINT ( 'NONE',  ( -9.072898850179999641, 36.94639249900000522, -148.2684494029999769 ) ) ;
#11848 = ORIENTED_EDGE ( 'NONE', *, *, #2280, .T. ) ;
#11849 = ADVANCED_FACE ( 'NONE', ( #7294 ), #3724, .T. ) ;
#11850 = CARTESIAN_POINT ( 'NONE',  ( -9.434278515689999978, -18.41834002140000237, -146.5552959529999839 ) ) ;
#11851 = MECHANICAL_DESIGN_GEOMETRIC_PRESENTATION_REPRESENTATION (  '', ( #18346 ), #6565 ) ;
#11852 = EDGE_CURVE ( 'NONE', #9023, #473, #1956, .T. ) ;
#11853 = VECTOR ( 'NONE', #7491, 1000.000000000000000 ) ;
#11854 = LINE ( 'NONE', #22690, #12505 ) ;
#11855 = CARTESIAN_POINT ( 'NONE',  ( 25.49993271304583331, 36.89748944256449192, -150.0552959529999839 ) ) ;
#11856 = ORIENTED_EDGE ( 'NONE', *, *, #11833, .F. ) ;
#11857 = EDGE_CURVE ( 'NONE', #11683, #1522, #21722, .T. ) ;
#11858 = B_SPLINE_CURVE_WITH_KNOTS ( 'NONE', 3,
 ( #5713, #14881, #6069, #22141, #5826, #721, #4051, #11284, #492, #7727 ),
 .UNSPECIFIED., .F., .F.,
 ( 4, 2, 2, 2, 4 ),
 ( 0.000000000000000000, 0.2500000000000000000, 0.5000000000000000000, 0.7500000000000000000, 1.000000000000000000 ),
 .UNSPECIFIED. ) ;
#11859 = EDGE_CURVE ( 'NONE', #2045, #14976, #160, .T. ) ;
#11860 = CARTESIAN_POINT ( 'NONE',  ( -17.71126569026348108, 40.30718541991128490, -145.9389846959304009 ) ) ;
#11861 = DIRECTION ( 'NONE',  ( 4.430318231639999944E-12, -6.100259101500000139E-13, 1.000000000000000000 ) ) ;
#11862 = ORIENTED_EDGE ( 'NONE', *, *, #16898, .T. ) ;
#11863 = DIRECTION ( 'NONE',  ( -2.808280234689999718E-18, 1.000000000000000000, 1.592654863659999653E-17 ) ) ;
#11864 = DIRECTION ( 'NONE',  ( 0.000000000000000000, 0.000000000000000000, 1.000000000000000000 ) ) ;
#11865 = EDGE_CURVE ( 'NONE', #1186, #6741, #23243, .T. ) ;
#11866 = ORIENTED_EDGE ( 'NONE', *, *, #13457, .T. ) ;
#11867 = FACE_OUTER_BOUND ( 'NONE', #22528, .T. ) ;
#11868 = DIRECTION ( 'NONE',  ( 0.000000000000000000, 0.000000000000000000, 1.000000000000000000 ) ) ;
#11869 = ORIENTED_EDGE ( 'NONE', *, *, #18529, .F. ) ;
#11870 = CARTESIAN_POINT ( 'NONE',  ( -14.97611052781801533, 40.21187687468054861, -142.1229170966665833 ) ) ;
#11871 = CARTESIAN_POINT ( 'NONE',  ( -25.73504040789999792, 33.16200571349999393, -143.7184748760000161 ) ) ;
#11872 = ORIENTED_EDGE ( 'NONE', *, *, #6702, .T. ) ;
#11873 = VECTOR ( 'NONE', #520, 1000.000000000000000 ) ;
#11874 = DIRECTION ( 'NONE',  ( 0.7071067811865474617, 0.7071067811865475727, 0.000000000000000000 ) ) ;
#11875 = EDGE_LOOP ( 'NONE', ( #18800, #2385, #6695, #19434 ) ) ;
#11876 = FACE_OUTER_BOUND ( 'NONE', #21972, .T. ) ;
#11877 = DIRECTION ( 'NONE',  ( 0.4860683305472111027, 0.8739208076473790054, -3.557471777477465713E-12 ) ) ;
#11878 = ORIENTED_EDGE ( 'NONE', *, *, #11865, .F. ) ;
#11879 = PLANE ( 'NONE',  #5319 ) ;
#11880 = ORIENTED_EDGE ( 'NONE', *, *, #6464, .T. ) ;
#11881 = PLANE ( 'NONE',  #14408 ) ;
#11882 = ORIENTED_EDGE ( 'NONE', *, *, #13526, .T. ) ;
#11883 = PRODUCT_DEFINITION_SHAPE ( 'NONE', 'NONE',  #1074 ) ;
#11884 = PRODUCT_DEFINITION_FORMATION_WITH_SPECIFIED_SOURCE ( 'ANY', '', #1629, .NOT_KNOWN. ) ;
#11885 = ORIENTED_EDGE ( 'NONE', *, *, #19045, .T. ) ;
#11886 = DIRECTION ( 'NONE',  ( -3.994014904670000134E-29, 1.000000000000000000, 0.000000000000000000 ) ) ;
#11887 = EDGE_CURVE ( 'NONE', #3797, #1160, #5263, .T. ) ;
#11888 = DIRECTION ( 'NONE',  ( -1.000000000000000000, 0.000000000000000000, 2.262368070660000099E-12 ) ) ;
#11889 = ADVANCED_FACE ( 'NONE', ( #1479 ), #8699, .F. ) ;
#11890 = LINE ( 'NONE', #6423, #7126 ) ;
#11891 = DIRECTION ( 'NONE',  ( -1.000000000000000000, 5.094701932209999624E-24, 2.257144641399999941E-12 ) ) ;
#11892 = ORIENTED_EDGE ( 'NONE', *, *, #11189, .T. ) ;
#11893 = CARTESIAN_POINT ( 'NONE',  ( -9.434278515689999978, -18.41834002140000237, -146.5552959529999839 ) ) ;
#11894 = DIRECTION ( 'NONE',  ( 1.000000000000000000, 0.000000000000000000, -2.257453483404482811E-12 ) ) ;
#11895 = CARTESIAN_POINT ( 'NONE',  ( 21.98914305888729714, -17.87864083493722944, -150.0552959529999839 ) ) ;
#11896 = CARTESIAN_POINT ( 'NONE',  ( -32.50000000000000000, -66.41770215440000413, -147.5656262009999864 ) ) ;
#11897 = LINE ( 'NONE', #19165, #441 ) ;
#11898 = DIRECTION ( 'NONE',  ( 0.000000000000000000, -1.000000000000000000, 0.000000000000000000 ) ) ;
#11899 = ORIENTED_EDGE ( 'NONE', *, *, #19332, .T. ) ;
#11900 = DIRECTION ( 'NONE',  ( -5.094701932209999624E-24, -1.000000000000000000, 1.149947916579999802E-35 ) ) ;
#11901 = CARTESIAN_POINT ( 'NONE',  ( -46.29070078840000235, 47.50000000000000000, -147.5552959529999839 ) ) ;
#11902 = LINE ( 'NONE', #21087, #5013 ) ;
#11903 = CARTESIAN_POINT ( 'NONE',  ( 27.68320006080000084, -32.50000000000000000, -148.5552959529999839 ) ) ;
#11904 = PRODUCT_DEFINITION_FORMATION_WITH_SPECIFIED_SOURCE ( 'ANY', '', #21028, .NOT_KNOWN. ) ;
#11905 = DIRECTION ( 'NONE',  ( -0.9954742291034677226, 0.09503188512734457583, 4.503697062742119365E-12 ) ) ;
#11906 = VERTEX_POINT ( 'NONE', #21822 ) ;
#11907 = CARTESIAN_POINT ( 'NONE',  ( -9.494338074862545440, 36.25121439520489730, -147.3777826702195739 ) ) ;
#11908 = DIRECTION ( 'NONE',  ( 0.9968185442904002880, -0.07970438983373201447, -8.712538262633510059E-14 ) ) ;
#11909 =( REPRESENTATION_RELATIONSHIP ('NONE','NONE', #7672, #16641 ) REPRESENTATION_RELATIONSHIP_WITH_TRANSFORMATION ( #21371 )SHAPE_REPRESENTATION_RELATIONSHIP( ) );
#11910 = CARTESIAN_POINT ( 'NONE',  ( -26.19803085470000070, 35.41001212129999942, -140.6029839040000127 ) ) ;
#11911 = EDGE_LOOP ( 'NONE', ( #3761, #19564, #21427, #16500, #15068 ) ) ;
#11912 =( BOUNDED_SURFACE ( )  B_SPLINE_SURFACE ( 5, 5, ( 
 ( #22035, #5723, #20257, #7157, #11181, #14301 ),
 ( #1595, #5497, #21695, #8816, #16092, #23348 ),
 ( #18232, #3710, #7038, #21572, #3478, #5253 ),
 ( #12504, #9165, #19786, #16445, #151, #10716 ),
 ( #1707, #14423, #12630, #19900, #3600, #10826 ),
 ( #18110, #1821, #9039, #16328, #36, #22151 ),
 ( #7965, #4524, #16901, #18805, #5952, #16666 ),
 ( #15001, #13442, #6079, #857, #8086, #11528 ),
 ( #15244, #11644, #7619, #15357, #18571, #22380 ) ),
 .UNSPECIFIED., .F., .F., .F. ) 
 B_SPLINE_SURFACE_WITH_KNOTS ( ( 6, 3, 6 ),
 ( 6, 6 ),
 ( 0.000000000000000000, 5.731822293570000504, 9.005131590149998644 ),
 ( 0.000000000000000000, 1.570796326823719946 ),
 .UNSPECIFIED. ) 
 GEOMETRIC_REPRESENTATION_ITEM ( )  RATIONAL_B_SPLINE_SURFACE ( (
 ( 1.000000000000000000, 0.5999999999926870498, 0.3999999999926869831, 0.2999999999945155427, 0.2499999999963435082, 0.2500000000000000000),
 ( 1.000000000000000000, 0.5999999999926870498, 0.3999999999926869831, 0.2999999999945155427, 0.2499999999963435082, 0.2500000000000000000),
 ( 1.000000000000000000, 0.5999999999926870498, 0.3999999999926869831, 0.2999999999945155427, 0.2499999999963435082, 0.2500000000000000000),
 ( 1.000000000000000000, 0.5999999999926870498, 0.3999999999926869831, 0.2999999999945155427, 0.2499999999963435082, 0.2500000000000000000),
 ( 1.000000000000000000, 0.5999999999926870498, 0.3999999999926869831, 0.2999999999945155427, 0.2499999999963435082, 0.2500000000000000000),
 ( 1.000000000000000000, 0.5999999999926870498, 0.3999999999926869831, 0.2999999999945155427, 0.2499999999963435082, 0.2500000000000000000),
 ( 1.000000000000000000, 0.5999999999926870498, 0.3999999999926869831, 0.2999999999945155427, 0.2499999999963435082, 0.2500000000000000000),
 ( 1.000000000000000000, 0.5999999999926870498, 0.3999999999926869831, 0.2999999999945155427, 0.2499999999963435082, 0.2500000000000000000),
 ( 1.000000000000000000, 0.5999999999926870498, 0.3999999999926869831, 0.2999999999945155427, 0.2499999999963435082, 0.2500000000000000000) ) ) 
 REPRESENTATION_ITEM ( '' )  SURFACE ( )  );
#11913 = CARTESIAN_POINT ( 'NONE',  ( 4.750000000030000002, -35.98606797749999942, -137.0552959530000123 ) ) ;
#11914 = CARTESIAN_POINT ( 'NONE',  ( -29.48665300989436844, 35.31333379408754780, -140.3895235765232030 ) ) ;
#11915 = DIRECTION ( 'NONE',  ( -2.257115129720000004E-12, 0.000000000000000000, -1.000000000000000000 ) ) ;
#11916 = VERTEX_POINT ( 'NONE', #18245 ) ;
#11917 = EDGE_CURVE ( 'NONE', #14539, #18280, #5506, .T. ) ;
#11918 = CARTESIAN_POINT ( 'NONE',  ( -13.62721142606643276, 36.29159090319166836, -140.6168710240230268 ) ) ;
#11919 = EDGE_CURVE ( 'NONE', #13247, #7407, #18297, .T. ) ;
#11920 = DIRECTION ( 'NONE',  ( 0.000000000000000000, 0.000000000000000000, 1.000000000000000000 ) ) ;
#11921 = CARTESIAN_POINT ( 'NONE',  ( -15.07147389515269431, 36.94622240755793996, -147.6034838243276681 ) ) ;
#11922 = FACE_OUTER_BOUND ( 'NONE', #12622, .T. ) ;
#11923 = CARTESIAN_POINT ( 'NONE',  ( -9.834719431799998191, 32.58365614919999587, -144.2353630830000100 ) ) ;
#11924 = EDGE_CURVE ( 'NONE', #10881, #8290, #13679, .T. ) ;
#11925 = CARTESIAN_POINT ( 'NONE',  ( -8.380324466120532279, 38.99863161821663482, -141.2713831690983568 ) ) ;
#11926 = AXIS2_PLACEMENT_3D ( 'NONE', #13573, #13700, #10114 ) ;
#11927 = VERTEX_POINT ( 'NONE', #16562 ) ;
#11928 = LINE ( 'NONE', #21111, #3082 ) ;
#11929 = ORIENTED_EDGE ( 'NONE', *, *, #1267, .F. ) ;
#11930 = CARTESIAN_POINT ( 'NONE',  ( -7.706057744118020025, 32.88414932266176294, -144.6585917708909790 ) ) ;
#11931 = CARTESIAN_POINT ( 'NONE',  ( -25.95437585259999835, 39.65968214939999825, -140.4458241780000094 ) ) ;
#11932 = LINE ( 'NONE', #5048, #174 ) ;
#11933 = ORIENTED_EDGE ( 'NONE', *, *, #11966, .F. ) ;
#11934 = CARTESIAN_POINT ( 'NONE',  ( 22.42370904790000097, -21.41421288319999761, -143.5552959529999839 ) ) ;
#11935 = CARTESIAN_POINT ( 'NONE',  ( 2.499999999879999990, -4.000000000000000000, -135.2552959529999725 ) ) ;
#11936 = VERTEX_POINT ( 'NONE', #2528 ) ;
#11937 = CARTESIAN_POINT ( 'NONE',  ( 7.683200060759999950, -21.50000000000000000, -138.5552959529999839 ) ) ;
#11938 = VECTOR ( 'NONE', #12846, 1000.000000000000000 ) ;
#11939 = CARTESIAN_POINT ( 'NONE',  ( -17.10091063371594089, 39.14571640553532461, -141.0837638240496119 ) ) ;
#11940 = CARTESIAN_POINT ( 'NONE',  ( -32.00000000000000000, 1.000000000000000000, -137.0552959530000123 ) ) ;
#11941 = CARTESIAN_POINT ( 'NONE',  ( 8.107579704549820576, 35.53766814163076759, -146.0852624393625092 ) ) ;
#11942 = DIRECTION ( 'NONE',  ( 2.257144641399999941E-12, 0.000000000000000000, 1.000000000000000000 ) ) ;
#11943 = CARTESIAN_POINT ( 'NONE',  ( -24.68545039255907625, 32.95552305825756889, -143.5792614360848347 ) ) ;
#11944 = CARTESIAN_POINT ( 'NONE',  ( -26.47299999999999898, 16.00000000000000000, -144.0552959529999839 ) ) ;
#11945 = EDGE_CURVE ( 'NONE', #6729, #14496, #624, .T. ) ;
#11946 = CARTESIAN_POINT ( 'NONE',  ( -11.48759298120159933, 37.74537190000896203, -140.3874188151567921 ) ) ;
#11947 = B_SPLINE_CURVE_WITH_KNOTS ( 'NONE', 3,
 ( #18698, #14653, #11068, #2408, #149, #611, #379, #12853, #16550, #20137 ),
 .UNSPECIFIED., .F., .F.,
 ( 4, 2, 2, 2, 4 ),
 ( 0.000000000000000000, 0.2500000000000000000, 0.5000000000000000000, 0.7500000000000000000, 1.000000000000000000 ),
 .UNSPECIFIED. ) ;
#11948 = ORIENTED_EDGE ( 'NONE', *, *, #16204, .T. ) ;
#11949 = PLANE ( 'NONE',  #15886 ) ;
#11951 = ORIENTED_EDGE ( 'NONE', *, *, #21042, .T. ) ;
#11950 = PRODUCT_DEFINITION ( 'UNKNOWN', '', #2801, #23035 ) ;
#11952 = LINE ( 'NONE', #8028, #4260 ) ;
#11953 = EDGE_LOOP ( 'NONE', ( #2563, #14849 ) ) ;
#11954 = CARTESIAN_POINT ( 'NONE',  ( 19.77963439039999827, 51.26338628509999751, -150.0552959529999839 ) ) ;
#11955 = EDGE_CURVE ( 'NONE', #3284, #1069, #392, .T. ) ;
#11956 = ORIENTED_EDGE ( 'NONE', *, *, #12977, .F. ) ;
#11957 = CIRCLE ( 'NONE', #19977, 2.500000000000000444 ) ;
#11958 = DIRECTION ( 'NONE',  ( 1.000000000000000000, 0.000000000000000000, -2.257120985840000117E-12 ) ) ;
#11959 = VERTEX_POINT ( 'NONE', #18816 ) ;
#11960 = ORIENTED_EDGE ( 'NONE', *, *, #18735, .T. ) ;
#11961 = CARTESIAN_POINT ( 'NONE',  ( -25.85824191589999899, -34.50000000000000000, -146.3157682190000060 ) ) ;
#11962 = CARTESIAN_POINT ( 'NONE',  ( 31.00000000000000000, 0.000000000000000000, -151.0552959529999839 ) ) ;
#11963 = CARTESIAN_POINT ( 'NONE',  ( -10.62000911041278783, 38.66961726526942300, -140.5822234582898886 ) ) ;
#11964 = CARTESIAN_POINT ( 'NONE',  ( -20.60824191589999899, -4.000000000000000000, -141.0657682190000060 ) ) ;
#11965 = PLANE ( 'NONE',  #3449 ) ;
#11966 = EDGE_CURVE ( 'NONE', #14263, #21289, #7855, .T. ) ;
#11967 = CARTESIAN_POINT ( 'NONE',  ( -9.771488485039439453, 38.65068379608815974, -147.6127673910835938 ) ) ;
#11968 = ORIENTED_EDGE ( 'NONE', *, *, #9382, .F. ) ;
#11969 = CARTESIAN_POINT ( 'NONE',  ( -9.157754307290000284, -15.75963164970000108, -147.5552959529999839 ) ) ;
#11970 = CARTESIAN_POINT ( 'NONE',  ( 9.770530770495106765, 36.20066385242879647, -146.4244424236570410 ) ) ;
#11971 = AXIS2_PLACEMENT_3D ( 'NONE', #16097, #10261, #23119 ) ;
#11972 = CARTESIAN_POINT ( 'NONE',  ( 19.13369214859999801, 50.50000000000000000, -136.0552959530000123 ) ) ;
#11973 = ADVANCED_FACE ( 'NONE', ( #22272 ), #23460, .F. ) ;
#11974 = VECTOR ( 'NONE', #19951, 1000.000000000000000 ) ;
#11975 = EDGE_LOOP ( 'NONE', ( #2586, #18078, #5546, #13182 ) ) ;
#11976 = LINE ( 'NONE', #16247, #22693 ) ;
#11977 = CARTESIAN_POINT ( 'NONE',  ( -23.51619327739999932, 36.94101002280000046, -140.1031831869999849 ) ) ;
#11978 = ORIENTED_EDGE ( 'NONE', *, *, #4757, .T. ) ;
#11979 = CARTESIAN_POINT ( 'NONE',  ( 19.00000000000000000, 33.50000000000000000, -137.0552959530000123 ) ) ;
#11980 = PLANE ( 'NONE',  #11216 ) ;
#11981 = ORIENTED_EDGE ( 'NONE', *, *, #19279, .T. ) ;
#11982 = CARTESIAN_POINT ( 'NONE',  ( 2.068499633510000102, -14.99362786250000035, -147.5552959529999839 ) ) ;
#11983 = ORIENTED_EDGE ( 'NONE', *, *, #9056, .T. ) ;
#11984 = DIRECTION ( 'NONE',  ( 1.000000000000000000, 0.000000000000000000, 0.000000000000000000 ) ) ;
#11985 = EDGE_CURVE ( 'NONE', #844, #11278, #15604, .T. ) ;
#11986 = CARTESIAN_POINT ( 'NONE',  ( -24.57863953938383972, 33.12365566000271855, -146.2648171788414118 ) ) ;
#11987 = ORIENTED_EDGE ( 'NONE', *, *, #4158, .T. ) ;
#11988 = PRODUCT ( 'Cover Plate', 'Cover Plate', '', ( #8844 ) ) ;
#11989 = EDGE_CURVE ( 'NONE', #2949, #4038, #6554, .T. ) ;
#11990 = FACE_OUTER_BOUND ( 'NONE', #16309, .T. ) ;
#11991 = ORIENTED_EDGE ( 'NONE', *, *, #10922, .T. ) ;
#11992 = DIRECTION ( 'NONE',  ( 0.000000000000000000, 0.000000000000000000, 1.000000000000000000 ) ) ;
#11993 = AXIS2_PLACEMENT_3D ( 'NONE', #18057, #1771, #21872 ) ;
#11994 = DIRECTION ( 'NONE',  ( 0.000000000000000000, -1.000000000000000000, 0.000000000000000000 ) ) ;
#11995 = VERTEX_POINT ( 'NONE', #8209 ) ;
#11996 = VECTOR ( 'NONE', #10256, 999.9999999999998863 ) ;
#11997 = FACE_OUTER_BOUND ( 'NONE', #14247, .T. ) ;
#11998 = ORIENTED_EDGE ( 'NONE', *, *, #5882, .F. ) ;
#11999 = EDGE_CURVE ( 'NONE', #10920, #1386, #21202, .T. ) ;
#12000 = DIRECTION ( 'NONE',  ( -0.9847555042252370550, 0.1739442350240419932, 1.095575354920264064E-14 ) ) ;
#12001 = ADVANCED_FACE ( 'NONE', ( #8095 ), #17625, .T. ) ;
#12002 = PLANE ( 'NONE',  #3765 ) ;
#12003 = ORIENTED_EDGE ( 'NONE', *, *, #10539, .F. ) ;
#12004 = ADVANCED_FACE ( 'NONE', ( #9991 ), #22737, .F. ) ;
#12005 = ADVANCED_FACE ( 'NONE', ( #6436 ), #20970, .T. ) ;
#12006 = VERTEX_POINT ( 'NONE', #2876 ) ;
#12007 = CARTESIAN_POINT ( 'NONE',  ( -7.500000000000000000, 25.50000000000000000, -150.0552959529999839 ) ) ;
#12008 = LINE ( 'NONE', #17490, #9673 ) ;
#12009 = CARTESIAN_POINT ( 'NONE',  ( -14.40871421779729111, 40.88007763208802459, -146.3531009209950469 ) ) ;
#12010 = PLANE ( 'NONE',  #14037 ) ;
#12011 = VECTOR ( 'NONE', #4875, 1000.000000000000000 ) ;
#12012 = ORIENTED_EDGE ( 'NONE', *, *, #10681, .T. ) ;
#12013 = VECTOR ( 'NONE', #15656, 1000.000000000000000 ) ;
#12014 = DIRECTION ( 'NONE',  ( 1.000000000000000000, -5.094701941669999797E-24, -2.257144641399999941E-12 ) ) ;
#12015 = CARTESIAN_POINT ( 'NONE',  ( 5.792747474879999636, -16.92794981449999980, -145.5552959529999839 ) ) ;
#12016 = CARTESIAN_POINT ( 'NONE',  ( 8.250000000030000891, -39.98606797749999942, -137.0552959530000123 ) ) ;
#12017 = CYLINDRICAL_SURFACE ( 'NONE', #77, 0.7500000000000006661 ) ;
#12018 = DIRECTION ( 'NONE',  ( 0.000000000000000000, 1.000000000000000000, 0.000000000000000000 ) ) ;
#12019 = ORIENTED_EDGE ( 'NONE', *, *, #22589, .F. ) ;
#12020 = CARTESIAN_POINT ( 'NONE',  ( -16.25499370519659692, 36.25618878915210530, -139.9176275600604242 ) ) ;
#12021 = CARTESIAN_POINT ( 'NONE',  ( 0.000000000000000000, 25.50000000000000000, -150.0552959529999839 ) ) ;
#12022 = DIRECTION ( 'NONE',  ( 1.526468026909999897E-13, 8.159623473500000156E-13, 1.000000000000000000 ) ) ;
#12023 = LINE ( 'NONE', #17507, #935 ) ;
#12024 = VERTEX_POINT ( 'NONE', #10108 ) ;
#12025 = CARTESIAN_POINT ( 'NONE',  ( -9.141321705204468628, 35.20952963915718215, -147.7046101278156129 ) ) ;
#12026 = CARTESIAN_POINT ( 'NONE',  ( -46.00000000000000000, 26.50000000000000000, -149.5552959529999839 ) ) ;
#12027 = ADVANCED_FACE ( 'NONE', ( #6668 ), #17382, .T. ) ;
#12028 = CIRCLE ( 'NONE', #18124, 2.999999999999999112 ) ;
#12029 = LINE ( 'NONE', #8566, #7522 ) ;
#12030 = EDGE_LOOP ( 'NONE', ( #10791, #4970, #3282, #22640 ) ) ;
#12031 = DIRECTION ( 'NONE',  ( -1.000000000000000000, 0.000000000000000000, 0.000000000000000000 ) ) ;
#12032 = CYLINDRICAL_SURFACE ( 'NONE', #20881, 1.500000000000001110 ) ;
#12033 = PLANE ( 'NONE',  #7938 ) ;
#12034 = ORIENTED_EDGE ( 'NONE', *, *, #14217, .F. ) ;
#12035 = CARTESIAN_POINT ( 'NONE',  ( -23.49616868971058281, 39.04951233234732655, -141.2607385382614495 ) ) ;
#12036 = CARTESIAN_POINT ( 'NONE',  ( 8.750000000030000891, -37.98606797749999942, -136.0552959530000123 ) ) ;
#12037 = DIRECTION ( 'NONE',  ( 0.000000000000000000, 1.000000000000000000, 2.257453483404482811E-12 ) ) ;
#12038 = DIRECTION ( 'NONE',  ( 2.257157423930000049E-12, 0.000000000000000000, 1.000000000000000000 ) ) ;
#12039 = VERTEX_POINT ( 'NONE', #18213 ) ;
#12040 = CARTESIAN_POINT ( 'NONE',  ( -6.033650297970000409, 36.94170754819999303, -147.9652040070000112 ) ) ;
#12041 = LINE ( 'NONE', #17884, #2506 ) ;
#12042 = VECTOR ( 'NONE', #13039, 1000.000000000000000 ) ;
#12043 = CARTESIAN_POINT ( 'NONE',  ( 9.167789811881178252, -37.80184220689855579, -150.0552959529999839 ) ) ;
#12044 = FACE_OUTER_BOUND ( 'NONE', #23507, .T. ) ;
#12045 = ORIENTED_EDGE ( 'NONE', *, *, #9148, .F. ) ;
#12046 = VECTOR ( 'NONE', #12773, 1000.000000000000000 ) ;
#12047 = CARTESIAN_POINT ( 'NONE',  ( -21.21916986627257273, 36.96385231547829164, -148.6710958206780617 ) ) ;
#12048 = ORIENTED_EDGE ( 'NONE', *, *, #4786, .T. ) ;
#12049 = CARTESIAN_POINT ( 'NONE',  ( -7.427142538590000065, 36.18616221519999954, -139.9783837409999876 ) ) ;
#12050 = PLANE ( 'NONE',  #3500 ) ;
#12051 = CARTESIAN_POINT ( 'NONE',  ( 11.57542696440981089, -21.02198665876327510, -148.5552959529999839 ) ) ;
#12052 = VERTEX_POINT ( 'NONE', #12614 ) ;
#12053 = EDGE_CURVE ( 'NONE', #2164, #3075, #12486, .T. ) ;
#12054 = FACE_OUTER_BOUND ( 'NONE', #19387, .T. ) ;
#12055 = PLANE ( 'NONE',  #7219 ) ;
#12056 = ORIENTED_EDGE ( 'NONE', *, *, #15044, .F. ) ;
#12057 = CARTESIAN_POINT ( 'NONE',  ( -20.92934595191639957, 38.39978090212863293, -147.3875924135098217 ) ) ;
#12058 = CIRCLE ( 'NONE', #4084, 2.500000000000000000 ) ;
#12059 = CARTESIAN_POINT ( 'NONE',  ( -17.53569647173340229, 40.68917497052807875, -144.4123951040356246 ) ) ;
#12060 = AXIS2_PLACEMENT_3D ( 'NONE', #22699, #2603, #8287 ) ;
#12061 = CARTESIAN_POINT ( 'NONE',  ( -14.21475634692216339, -40.07808196999505412, -150.0552959529999839 ) ) ;
#12062 = FACE_OUTER_BOUND ( 'NONE', #7841, .T. ) ;
#12063 = CARTESIAN_POINT ( 'NONE',  ( 12.50000000020000002, 20.50000000000000000, -136.5552959530000123 ) ) ;
#12064 = CARTESIAN_POINT ( 'NONE',  ( -24.26662447760775976, 35.20109951628700173, -148.0073960933498256 ) ) ;
#12065 = CARTESIAN_POINT ( 'NONE',  ( -3.499999999969999998, 46.50000000000000000, -136.5552959530000123 ) ) ;
#12066 = FACE_OUTER_BOUND ( 'NONE', #167, .T. ) ;
#12067 = ORIENTED_EDGE ( 'NONE', *, *, #16098, .T. ) ;
#12068 = DIRECTION ( 'NONE',  ( 1.457985068979999943E-12, -1.723073263340000007E-12, -1.000000000000000000 ) ) ;
#12069 = PRODUCT_DEFINITION_CONTEXT ( 'detailed design', #7051, 'design' ) ;
#12071 = VERTEX_POINT ( 'NONE', #7141 ) ;
#12070 = CIRCLE ( 'NONE', #4468, 2.000000000000000000 ) ;
#12072 = ORIENTED_EDGE ( 'NONE', *, *, #13409, .F. ) ;
#12073 = CIRCLE ( 'NONE', #4872, 9.000000000000000000 ) ;
#12074 = ORIENTED_EDGE ( 'NONE', *, *, #4059, .F. ) ;
#12075 = CARTESIAN_POINT ( 'NONE',  ( 31.50000000000000000, 40.03620104880000241, -136.5552959530000123 ) ) ;
#12076 = CARTESIAN_POINT ( 'NONE',  ( -28.67645553090000021, 33.79622934780000065, -142.1760638819999940 ) ) ;
#12077 = VERTEX_POINT ( 'NONE', #5014 ) ;
#12078 = VERTEX_POINT ( 'NONE', #5234 ) ;
#12079 = EDGE_CURVE ( 'NONE', #20700, #22206, #21738, .T. ) ;
#12080 = DIRECTION ( 'NONE',  ( -2.602084704489999637E-17, 1.000000000000000000, 4.426606872070000353E-37 ) ) ;
#12081 = CARTESIAN_POINT ( 'NONE',  ( -19.24427237058737106, 36.32221599350456387, -147.8366771256798131 ) ) ;
#12082 = PLANE ( 'NONE',  #12250 ) ;
#12083 = EDGE_CURVE ( 'NONE', #6228, #14075, #9545, .T. ) ;
#12084 = CARTESIAN_POINT ( 'NONE',  ( -12.02450515616398086, 36.94061592733338983, -147.5849826168277730 ) ) ;
#12085 = LINE ( 'NONE', #17212, #13702 ) ;
#12086 = CARTESIAN_POINT ( 'NONE',  ( -10.03947840059807817, 37.95006096691596298, -148.1887910594758750 ) ) ;
#12087 = EDGE_LOOP ( 'NONE', ( #17822, #4906, #1930, #3775, #10297, #4855, #16815, #23483, #6013, #2487, #3469, #17381, #5780, #677, #21647, #8208, #4601, #559, #237, #22601, #11420, #7929, #14051, #9061, #18100, #3872, #9457, #12224, #19284, #1284, #9630, #5428 ) ) ;
#12088 = CARTESIAN_POINT ( 'NONE',  ( -28.03429568389999815, 32.40695676820000415, -144.4586890250000124 ) ) ;
#12089 = VECTOR ( 'NONE', #29, 1000.000000000000000 ) ;
#12090 = CARTESIAN_POINT ( 'NONE',  ( 19.13369214859999801, -51.00000000000000000, -150.0552959529999839 ) ) ;
#12091 = AXIS2_PLACEMENT_3D ( 'NONE', #7717, #7483, #5934 ) ;
#12092 = DIRECTION ( 'NONE',  ( -0.1000233216789610108, -0.9949850929136109245, 3.591470555298595137E-13 ) ) ;
#12093 = EDGE_LOOP ( 'NONE', ( #22018, #5180, #6515, #19670 ) ) ;
#12094 = CIRCLE ( 'NONE', #17438, 35.00000000000000000 ) ;
#12095 = DIRECTION ( 'NONE',  ( -0.9753087663813413410, 0.2208456705930775810, 8.935806277123132252E-12 ) ) ;
#12096 = ORIENTED_EDGE ( 'NONE', *, *, #2829, .F. ) ;
#12097 = DIRECTION ( 'NONE',  ( 0.000000000000000000, 0.000000000000000000, -1.000000000000000000 ) ) ;
#12098 = CARTESIAN_POINT ( 'NONE',  ( -21.35824191589999899, -4.750000000000000000, -146.3157682190075093 ) ) ;
#12099 = EDGE_CURVE ( 'NONE', #23414, #4587, #17980, .T. ) ;
#12100 = ORIENTED_EDGE ( 'NONE', *, *, #11697, .F. ) ;
#12101 = CYLINDRICAL_SURFACE ( 'NONE', #20521, 1.000000000000004219 ) ;
#12102 = CARTESIAN_POINT ( 'NONE',  ( 10.50000000020000002, 20.50000000000000000, -136.5552959530000123 ) ) ;
#12103 = ORIENTED_EDGE ( 'NONE', *, *, #5041, .T. ) ;
#12104 = CARTESIAN_POINT ( 'NONE',  ( -15.13725729890880878, 41.64066907640037130, -144.4902128453323655 ) ) ;
#12105 = CARTESIAN_POINT ( 'NONE',  ( -25.19866427022423494, 35.19115820926130311, -148.3071468095327816 ) ) ;
#12106 = ORIENTED_EDGE ( 'NONE', *, *, #16732, .F. ) ;
#12107 = VECTOR ( 'NONE', #11121, 1000.000000000000000 ) ;
#12108 = EDGE_LOOP ( 'NONE', ( #14093, #8538, #9387, #23213, #21240, #17187, #671 ) ) ;
#12109 = CYLINDRICAL_SURFACE ( 'NONE', #362, 9.000000000000000000 ) ;
#12110 = AXIS2_PLACEMENT_3D ( 'NONE', #2701, #22926, #15190 ) ;
#12111 = DIRECTION ( 'NONE',  ( 1.190078432789999897E-50, 1.000000000000000000, 0.000000000000000000 ) ) ;
#12112 = ORIENTED_EDGE ( 'NONE', *, *, #2362, .F. ) ;
#12113 = ADVANCED_FACE ( 'NONE', ( #19886 ), #12256, .F. ) ;
#12114 = CARTESIAN_POINT ( 'NONE',  ( 24.11847952820000174, -31.58456057200000089, -143.5552959529999839 ) ) ;
#12115 = VECTOR ( 'NONE', #8070, 1000.000000000000000 ) ;
#12116 = CIRCLE ( 'NONE', #11729, 4.000000000000003553 ) ;
#12117 = FACE_OUTER_BOUND ( 'NONE', #23183, .T. ) ;
#12118 = CARTESIAN_POINT ( 'NONE',  ( 18.95053822279999878, 50.00000000000000000, -151.0552959529999839 ) ) ;
#12119 = EDGE_CURVE ( 'NONE', #14496, #1756, #10457, .T. ) ;
#12120 = VERTEX_POINT ( 'NONE', #8911 ) ;
#12121 = CARTESIAN_POINT ( 'NONE',  ( 7.421918030004944988, -2.714756346922159835, -150.0552959530000123 ) ) ;
#12122 = VECTOR ( 'NONE', #1115, 1000.000000000000000 ) ;
#12123 = CARTESIAN_POINT ( 'NONE',  ( -21.93648690847361138, 37.04947573026748131, -148.4875734863013008 ) ) ;
#12124 = CARTESIAN_POINT ( 'NONE',  ( -13.66607852796262357, 39.56920417019204450, -140.6329893835133475 ) ) ;
#12125 = LINE ( 'NONE', #12603, #3789 ) ;
#12126 = ORIENTED_EDGE ( 'NONE', *, *, #9010, .F. ) ;
#12127 = PLANE ( 'NONE',  #9009 ) ;
#12128 = DIRECTION ( 'NONE',  ( 1.000000000000000000, 0.000000000000000000, -2.245315046049999660E-12 ) ) ;
#12129 = AXIS2_PLACEMENT_3D ( 'NONE', #3399, #23394, #8616 ) ;
#12130 = EDGE_CURVE ( 'NONE', #2045, #17877, #7380, .T. ) ;
#12131 = DIRECTION ( 'NONE',  ( 0.000000000000000000, -1.000000000000000000, 3.568879590630000244E-13 ) ) ;
#12132 = LINE ( 'NONE', #15949, #1844 ) ;
#12133 = LINE ( 'NONE', #6313, #20967 ) ;
#12134 = VECTOR ( 'NONE', #20112, 1000.000000000000000 ) ;
#12135 = CARTESIAN_POINT ( 'NONE',  ( -13.86630785140000022, 51.50000000000000000, -136.0552959530000123 ) ) ;
#12136 = EDGE_CURVE ( 'NONE', #1659, #11473, #21436, .T. ) ;
#12137 = VERTEX_POINT ( 'NONE', #10809 ) ;
#12138 = CARTESIAN_POINT ( 'NONE',  ( -16.20147620265711907, 33.40528963980359833, -143.4816615022452027 ) ) ;
#12139 = EDGE_CURVE ( 'NONE', #1369, #14338, #14404, .T. ) ;
#12140 = LINE ( 'NONE', #12021, #6802 ) ;
#12141 = EDGE_CURVE ( 'NONE', #4200, #19696, #1449, .T. ) ;
#12142 = CARTESIAN_POINT ( 'NONE',  ( -5.459597139290000456, 36.94776568910000236, -139.8191173760000083 ) ) ;
#12143 = CARTESIAN_POINT ( 'NONE',  ( -7.706057744120000663, 32.88414932280000613, -144.6585917709999762 ) ) ;
#12144 = CARTESIAN_POINT ( 'NONE',  ( 7.935413903360000631, 38.54667735430000164, -117.9621819409999972 ) ) ;
#12145 = EDGE_LOOP ( 'NONE', ( #15843, #18168 ) ) ;
#12146 = FACE_OUTER_BOUND ( 'NONE', #12591, .T. ) ;
#12147 = CARTESIAN_POINT ( 'NONE',  ( -46.00000000000000000, 47.50000000000000000, -149.0552959529999839 ) ) ;
#12148 = ORIENTED_EDGE ( 'NONE', *, *, #3436, .T. ) ;
#12149 = VECTOR ( 'NONE', #12251, 1000.000000000000000 ) ;
#12150 = AXIS2_PLACEMENT_3D ( 'NONE', #19199, #17062, #8126 ) ;
#12151 = AXIS2_PLACEMENT_3D ( 'NONE', #10856, #14679, #18261 ) ;
#12152 = VECTOR ( 'NONE', #12587, 1000.000000000000000 ) ;
#12153 = CARTESIAN_POINT ( 'NONE',  ( -29.26469713025206687, 35.46669211296976698, -140.6743228978359923 ) ) ;
#12154 = DIRECTION ( 'NONE',  ( 1.000000000000000000, 0.000000000000000000, -2.257171095940000041E-12 ) ) ;
#12155 = VERTEX_POINT ( 'NONE', #9024 ) ;
#12156 = ADVANCED_FACE ( 'NONE', ( #9149 ), #19531, .T. ) ;
#12157 = CARTESIAN_POINT ( 'NONE',  ( -24.05878554920779777, 40.01929703906174751, -145.8416302223327818 ) ) ;
#12158 = DIRECTION ( 'NONE',  ( 0.000000000000000000, 4.009147065150000317E-51, -1.000000000000000000 ) ) ;
#12159 = CARTESIAN_POINT ( 'NONE',  ( 22.32684911886484613, -15.33692515329977546, -144.5552959530006945 ) ) ;
#12160 = LINE ( 'NONE', #13592, #22769 ) ;
#12161 = VERTEX_POINT ( 'NONE', #16310 ) ;
#12162 = CARTESIAN_POINT ( 'NONE',  ( -10.47418533528157880, 33.50012463732112167, -145.9259304110134110 ) ) ;
#12163 = FACE_OUTER_BOUND ( 'NONE', #674, .T. ) ;
#12164 = EDGE_CURVE ( 'NONE', #18803, #21084, #16432, .T. ) ;
#12165 = CARTESIAN_POINT ( 'NONE',  ( -9.389499115902607329, 36.98418387199379254, -147.3811924090304046 ) ) ;
#12166 = DIRECTION ( 'NONE',  ( 0.7633862853691523176, 0.6459422414661291079, 0.000000000000000000 ) ) ;
#12167 = ORIENTED_EDGE ( 'NONE', *, *, #5142, .T. ) ;
#12168 = EDGE_CURVE ( 'NONE', #1863, #8058, #20, .T. ) ;
#12169 = AXIS2_PLACEMENT_3D ( 'NONE', #7023, #3463, #10932 ) ;
#12170 = AXIS2_PLACEMENT_3D ( 'NONE', #5276, #19921, #1730 ) ;
#12171 = CARTESIAN_POINT ( 'NONE',  ( -3.500000000000000000, 44.50000000000000000, -151.0552959529999839 ) ) ;
#12172 = ORIENTED_EDGE ( 'NONE', *, *, #6903, .F. ) ;
#12173 = CARTESIAN_POINT ( 'NONE',  ( -7.107905118343079920, 36.22301459074771657, -148.1570340891202022 ) ) ;
#12174 = FACE_OUTER_BOUND ( 'NONE', #17657, .T. ) ;
#12175 = CARTESIAN_POINT ( 'NONE',  ( -4.521812268189999706, -27.38504028299999860, -148.5552959529999839 ) ) ;
#12176 = ORIENTED_EDGE ( 'NONE', *, *, #17107, .T. ) ;
#12177 = CARTESIAN_POINT ( 'NONE',  ( -7.002253344594251416, -25.58393298470214816, -143.5552959529972554 ) ) ;
#12178 = FACE_OUTER_BOUND ( 'NONE', #4829, .T. ) ;
#12179 = MANIFOLD_SOLID_BREP ( 'lock_assembly.1\\lock body.2\\PartBody', #17147 ) ;
#12180 = ORIENTED_EDGE ( 'NONE', *, *, #12992, .T. ) ;
#12181 = CARTESIAN_POINT ( 'NONE',  ( -30.49999999990000177, 26.50000000000000000, -147.5552959529999839 ) ) ;
#12182 = CARTESIAN_POINT ( 'NONE',  ( 17.88080765318374077, 24.01462304344178023, -150.0552959529999839 ) ) ;
#12183 = PLANE ( 'NONE',  #20384 ) ;
#12184 = DIRECTION ( 'NONE',  ( 0.000000000000000000, -1.000000000000000000, 8.159623473500000156E-13 ) ) ;
#12185 = AXIS2_PLACEMENT_3D ( 'NONE', #9761, #13466, #11666 ) ;
#12186 = CARTESIAN_POINT ( 'NONE',  ( -18.07392865170000107, -1.500000000000000000, -146.3157682190000060 ) ) ;
#12187 = CARTESIAN_POINT ( 'NONE',  ( -16.13502618060000060, 32.80445174449999968, -146.2787800969999807 ) ) ;
#12188 = DIRECTION ( 'NONE',  ( -1.000000000000000000, 0.000000000000000000, 2.257120985840000117E-12 ) ) ;
#12189 = CARTESIAN_POINT ( 'NONE',  ( 8.750000000030000891, -39.98606797749999942, -136.0552959530000123 ) ) ;
#12190 = EDGE_CURVE ( 'NONE', #4104, #16441, #22468, .T. ) ;
#12191 = ORIENTED_EDGE ( 'NONE', *, *, #10532, .T. ) ;
#12192 = EDGE_CURVE ( 'NONE', #22451, #8268, #2046, .T. ) ;
#12193 = FACE_OUTER_BOUND ( 'NONE', #14699, .T. ) ;
#12194 =( BOUNDED_SURFACE ( )  B_SPLINE_SURFACE ( 5, 5, ( 
 ( #14377, #18306, #3788, #21882, #11030, #10549 ),
 ( #17830, #3557, #12701, #7241, #8770, #5341 ),
 ( #1551, #16048, #10784, #21769, #12583, #19858 ),
 ( #16167, #9001, #3435, #23307, #7000, #14261 ),
 ( #114, #5456, #21526, #12460, #19968, #10670 ),
 ( #1666, #10904, #3670, #1899, #9124, #17953 ),
 ( #8888, #21988, #22333, #16741, #11599, #22452 ),
 ( #686, #18874, #18764, #5678, #20433, #6025 ),
 ( #2123, #22220, #7916, #20669, #14850, #3907 ),
 ( #9345, #22106, #4362, #5910, #2587, #13399 ),
 ( #454, #5794, #13279, #15195, #2475, #6148 ),
 ( #15073, #13054, #9814, #18521, #4251, #16859 ) ),
 .UNSPECIFIED., .F., .F., .F. ) 
 B_SPLINE_SURFACE_WITH_KNOTS ( ( 6, 3, 3, 6 ),
 ( 6, 6 ),
 ( 0.000000000000000000, 4.469553974960000176, 8.969854531369998440, 13.50363095830000049 ),
 ( 0.000000000000000000, 1.570796327036555029 ),
 .UNSPECIFIED. ) 
 GEOMETRIC_REPRESENTATION_ITEM ( )  RATIONAL_B_SPLINE_SURFACE ( (
 ( 1.000000000000000000, 0.5999999999384889593, 0.3999999999384890037, 0.2999999999538665030, 0.2499999999692444907, 0.2500000000000000000),
 ( 1.000000000000000000, 0.5999999999384889593, 0.3999999999384890037, 0.2999999999538665030, 0.2499999999692444907, 0.2500000000000000000),
 ( 1.000000000000000000, 0.5999999999384889593, 0.3999999999384890037, 0.2999999999538665030, 0.2499999999692444907, 0.2500000000000000000),
 ( 1.000000000000000000, 0.5999999999384889593, 0.3999999999384890037, 0.2999999999538665030, 0.2499999999692444907, 0.2500000000000000000),
 ( 1.000000000000000000, 0.5999999999384889593, 0.3999999999384890037, 0.2999999999538665030, 0.2499999999692444907, 0.2500000000000000000),
 ( 1.000000000000000000, 0.5999999999384889593, 0.3999999999384890037, 0.2999999999538665030, 0.2499999999692444907, 0.2500000000000000000),
 ( 1.000000000000000000, 0.5999999999384889593, 0.3999999999384890037, 0.2999999999538665030, 0.2499999999692444907, 0.2500000000000000000),
 ( 1.000000000000000000, 0.5999999999384889593, 0.3999999999384890037, 0.2999999999538665030, 0.2499999999692444907, 0.2500000000000000000),
 ( 1.000000000000000000, 0.5999999999384889593, 0.3999999999384890037, 0.2999999999538665030, 0.2499999999692444907, 0.2500000000000000000),
 ( 1.000000000000000000, 0.5999999999384889593, 0.3999999999384890037, 0.2999999999538665030, 0.2499999999692444907, 0.2500000000000000000),
 ( 1.000000000000000000, 0.5999999999384889593, 0.3999999999384890037, 0.2999999999538665030, 0.2499999999692444907, 0.2500000000000000000),
 ( 1.000000000000000000, 0.5999999999384889593, 0.3999999999384890037, 0.2999999999538665030, 0.2499999999692444907, 0.2500000000000000000) ) ) 
 REPRESENTATION_ITEM ( '' )  SURFACE ( )  );
#12195 = ORIENTED_EDGE ( 'NONE', *, *, #19999, .F. ) ;
#12196 = FILL_AREA_STYLE ('',( #15773 ) ) ;
#12197 = EDGE_LOOP ( 'NONE', ( #15461, #9118, #3189, #18520, #22963, #10277, #8438, #8875 ) ) ;
#12198 = DIRECTION ( 'NONE',  ( 1.000000000000000000, 0.000000000000000000, 0.000000000000000000 ) ) ;
#12199 = CARTESIAN_POINT ( 'NONE',  ( -28.53262905876626121, 34.95472962840860021, -141.1599551600052109 ) ) ;
#12200 = VERTEX_POINT ( 'NONE', #5709 ) ;
#12201 = AXIS2_PLACEMENT_3D ( 'NONE', #14600, #12921, #18401 ) ;
#12202 = VECTOR ( 'NONE', #16710, 1000.000000000000000 ) ;
#12203 = CIRCLE ( 'NONE', #15255, 2.500000000000000444 ) ;
#12204 = EDGE_LOOP ( 'NONE', ( #14658, #15535, #5871, #11273 ) ) ;
#12205 = DIRECTION ( 'NONE',  ( 0.000000000000000000, 0.000000000000000000, 1.000000000000000000 ) ) ;
#12206 = CARTESIAN_POINT ( 'NONE',  ( -18.18930989820000121, 36.96028804430000037, -147.6841622079999752 ) ) ;
#12207 = FACE_OUTER_BOUND ( 'NONE', #22500, .T. ) ;
#12208 = FACE_OUTER_BOUND ( 'NONE', #3316, .T. ) ;
#12209 = CARTESIAN_POINT ( 'NONE',  ( -6.932379827013399165, 32.27029367454267827, -144.6524339332874263 ) ) ;
#12210 = EDGE_LOOP ( 'NONE', ( #14021, #1774, #7214, #5803 ) ) ;
#12211 = CARTESIAN_POINT ( 'NONE',  ( 1.133692148550000001, -51.50000000000000000, -136.0552959530000123 ) ) ;
#12212 = LINE ( 'NONE', #19491, #2642 ) ;
#12213 = CARTESIAN_POINT ( 'NONE',  ( -21.35824191589999899, -4.750000000000000000, -144.8157682190000060 ) ) ;
#12214 = VECTOR ( 'NONE', #5117, 1000.000000000000000 ) ;
#12215 = ORIENTED_EDGE ( 'NONE', *, *, #12272, .T. ) ;
#12216 = AXIS2_PLACEMENT_3D ( 'NONE', #18362, #22276, #20379 ) ;
#12217 = AXIS2_PLACEMENT_3D ( 'NONE', #16252, #14690, #1986 ) ;
#12218 = EDGE_CURVE ( 'NONE', #18451, #7409, #7604, .T. ) ;
#12219 = DIRECTION ( 'NONE',  ( 1.000000000000000000, 0.000000000000000000, 2.516505522483685870E-12 ) ) ;
#12220 = EDGE_LOOP ( 'NONE', ( #22031, #19699, #9489, #15160, #8819, #2288, #922 ) ) ;
#12221 = CARTESIAN_POINT ( 'NONE',  ( -20.84101097270000125, 38.55092845019999714, -147.7610021339999946 ) ) ;
#12222 = EDGE_CURVE ( 'NONE', #17568, #9455, #9498, .T. ) ;
#12223 = DIRECTION ( 'NONE',  ( 0.7633862853691524286, 0.6459422414661292189, -5.800915303671161101E-15 ) ) ;
#12224 = ORIENTED_EDGE ( 'NONE', *, *, #10061, .T. ) ;
#12225 = FACE_BOUND ( 'NONE', #1751, .T. ) ;
#12226 = EDGE_LOOP ( 'NONE', ( #17923, #16083, #15944, #11740 ) ) ;
#12227 = CARTESIAN_POINT ( 'NONE',  ( -15.26331651089999930, 39.75437292659999855, -147.8043400740000095 ) ) ;
#12228 = DIRECTION ( 'NONE',  ( 1.527666881879999979E-13, 8.171241461240000022E-13, 1.000000000000000000 ) ) ;
#12229 = ORIENTED_EDGE ( 'NONE', *, *, #3157, .T. ) ;
#12230 = ORIENTED_EDGE ( 'NONE', *, *, #22174, .F. ) ;
#12231 = DIRECTION ( 'NONE',  ( -0.07970438983373200059, -0.9968185442904001770, 8.242295734823311485E-13 ) ) ;
#12232 = CARTESIAN_POINT ( 'NONE',  ( 8.900000000049999471, 37.00000000000000000, -148.7552959530000010 ) ) ;
#12233 = ORIENTED_EDGE ( 'NONE', *, *, #22879, .T. ) ;
#12234 = AXIS2_PLACEMENT_3D ( 'NONE', #8993, #21285, #21762 ) ;
#12235 = DIRECTION ( 'NONE',  ( 1.000000000000000000, 0.000000000000000000, -2.257453483404485639E-12 ) ) ;
#12236 = CIRCLE ( 'NONE', #13001, 1.500000000000001332 ) ;
#12237 = AXIS2_PLACEMENT_3D ( 'NONE', #20328, #11144, #11370 ) ;
#12238 = CARTESIAN_POINT ( 'NONE',  ( -34.61111111099999960, 29.00000000000000000, -140.5552959529999839 ) ) ;
#12239 = CARTESIAN_POINT ( 'NONE',  ( -8.770737564319999180, -11.35481373070000011, -144.5552959529999839 ) ) ;
#12240 = ORIENTED_EDGE ( 'NONE', *, *, #19289, .F. ) ;
#12241 = LINE ( 'NONE', #10444, #21936 ) ;
#12242 = CARTESIAN_POINT ( 'NONE',  ( 15.85402906740000084, -26.57485422999999969, -145.5552959529999839 ) ) ;
#12243 = CARTESIAN_POINT ( 'NONE',  ( -14.45813593939999997, 41.09907220950000095, -141.6721478100000127 ) ) ;
#12244 = FACE_OUTER_BOUND ( 'NONE', #11975, .T. ) ;
#12245 = EDGE_LOOP ( 'NONE', ( #15154, #11725, #13445, #12569 ) ) ;
#12246 = SURFACE_STYLE_USAGE ( .BOTH. , #5113 ) ;
#12247 = MECHANICAL_DESIGN_GEOMETRIC_PRESENTATION_REPRESENTATION (  '', ( #13017 ), #13777 ) ;
#12248 = ADVANCED_FACE ( 'NONE', ( #16770 ), #7948, .F. ) ;
#12249 = DIRECTION ( 'NONE',  ( 1.000000000000000000, -5.094701941669999797E-24, -2.257144641399999941E-12 ) ) ;
#12250 = AXIS2_PLACEMENT_3D ( 'NONE', #11601, #6378, #2940 ) ;
#12251 = DIRECTION ( 'NONE',  ( 0.000000000000000000, 1.000000000000000000, 0.000000000000000000 ) ) ;
#12252 = CARTESIAN_POINT ( 'NONE',  ( 17.45728951470000112, -20.98759093920000041, -146.5552959529999839 ) ) ;
#12253 = CARTESIAN_POINT ( 'NONE',  ( -46.00000000000000000, 47.50000000000000000, -149.5552959529999839 ) ) ;
#12254 = DIRECTION ( 'NONE',  ( 1.527666881879999979E-13, 8.171241461240000022E-13, 1.000000000000000000 ) ) ;
#12255 = ORIENTED_EDGE ( 'NONE', *, *, #21833, .T. ) ;
#12256 = PLANE ( 'NONE',  #2722 ) ;
#12257 = LINE ( 'NONE', #21911, #17888 ) ;
#12258 = CARTESIAN_POINT ( 'NONE',  ( 1.000000000160000013, 41.50000000000000000, -139.5552959529999839 ) ) ;
#12259 = ADVANCED_FACE ( 'NONE', ( #7721 ), #4766, .F. ) ;
#12260 = LINE ( 'NONE', #17387, #16796 ) ;
#12261 = CARTESIAN_POINT ( 'NONE',  ( -7.010349701930000066, 37.05829245179999987, -148.1453878979999956 ) ) ;
#12262 = LINE ( 'NONE', #15960, #16121 ) ;
#12263 = ORIENTED_EDGE ( 'NONE', *, *, #14108, .T. ) ;
#12264 = CARTESIAN_POINT ( 'NONE',  ( 13.13369214859999978, -51.50000000000000000, -136.0552959530000123 ) ) ;
#12265 = CARTESIAN_POINT ( 'NONE',  ( -3.499999999959999997, 40.00000000000000000, -153.0552959529999839 ) ) ;
#12266 = ORIENTED_EDGE ( 'NONE', *, *, #109, .T. ) ;
#12267 = EDGE_CURVE ( 'NONE', #10772, #13630, #1389, .T. ) ;
#12268 = CARTESIAN_POINT ( 'NONE',  ( 6.500000000170000014, 16.50000000000000000, -136.5552959530000123 ) ) ;
#12269 = DIRECTION ( 'NONE',  ( 0.000000000000000000, -4.148443855749999753E-27, -1.000000000000000000 ) ) ;
#12270 = VERTEX_POINT ( 'NONE', #21496 ) ;
#12271 = LINE ( 'NONE', #15971, #18592 ) ;
#12272 = EDGE_CURVE ( 'NONE', #3235, #9183, #8737, .T. ) ;
#12273 = DIRECTION ( 'NONE',  ( 4.510774274160000731E-12, -1.321907670990000086E-13, 1.000000000000000000 ) ) ;
#12274 = CARTESIAN_POINT ( 'NONE',  ( 17.66940543669999997, -18.68690163239999791, -145.5552959529999839 ) ) ;
#12275 = CARTESIAN_POINT ( 'NONE',  ( 7.038350098255955700, 36.65929791540875016, -141.5783375516163005 ) ) ;
#12276 = VERTEX_POINT ( 'NONE', #15668 ) ;
#12277 = FACE_OUTER_BOUND ( 'NONE', #20806, .T. ) ;
#12278 = CARTESIAN_POINT ( 'NONE',  ( -32.50000000000000000, -35.00000000000000000, -140.0552959529999839 ) ) ;
#12279 = CYLINDRICAL_SURFACE ( 'NONE', #13588, 7.500000000000005329 ) ;
#12280 = CARTESIAN_POINT ( 'NONE',  ( 8.750000000030000891, -35.98606797749999942, -136.0552959530000123 ) ) ;
#12281 = ORIENTED_EDGE ( 'NONE', *, *, #15129, .F. ) ;
#12282 = CARTESIAN_POINT ( 'NONE',  ( -6.477935707790000386, -19.20465386649999928, -147.5552959529999839 ) ) ;
#12283 = SURFACE_STYLE_USAGE ( .BOTH. , #17293 ) ;
#12284 = B_SPLINE_CURVE_WITH_KNOTS ( 'NONE', 3,
 ( #1999, #5308, #10764, #11342, #20650, #11120, #16840, #18854, #18628, #2343 ),
 .UNSPECIFIED., .F., .F.,
 ( 4, 2, 2, 2, 4 ),
 ( 0.000000000000000000, 0.2500000000000000000, 0.5000000000000000000, 0.7500000000000000000, 1.000000000000000000 ),
 .UNSPECIFIED. ) ;
#12285 = EDGE_CURVE ( 'NONE', #14669, #1892, #19478, .T. ) ;
#12286 = EDGE_LOOP ( 'NONE', ( #7299, #23384, #21689, #200 ) ) ;
#12287 = CARTESIAN_POINT ( 'NONE',  ( -7.998490025638652412, 36.27838346975144646, -140.7398725790258993 ) ) ;
#12288 = CARTESIAN_POINT ( 'NONE',  ( -22.83308877300000006, 39.55027303330000166, -140.7145628009999996 ) ) ;
#12289 = CARTESIAN_POINT ( 'NONE',  ( 32.50000000000000000, 32.96379895120000469, -137.0552959530000123 ) ) ;
#12290 = EDGE_CURVE ( 'NONE', #13032, #21821, #22930, .T. ) ;
#12291 = VERTEX_POINT ( 'NONE', #15889 ) ;
#12292 = LINE ( 'NONE', #12525, #21291 ) ;
#12293 = LINE ( 'NONE', #10848, #11372 ) ;
#12294 = ORIENTED_EDGE ( 'NONE', *, *, #4659, .F. ) ;
#12295 = DIRECTION ( 'NONE',  ( -0.1736481776649230480, 0.000000000000000000, 0.9848077530125620704 ) ) ;
#12296 = EDGE_CURVE ( 'NONE', #12161, #14060, #3172, .T. ) ;
#12297 = CARTESIAN_POINT ( 'NONE',  ( 2.139623390130000136, -12.81320239329999922, -143.5552959529999839 ) ) ;
#12298 = EDGE_CURVE ( 'NONE', #6401, #21209, #4832, .T. ) ;
#12299 = CARTESIAN_POINT ( 'NONE',  ( -17.62135916506278122, -41.48914305888730780, -150.0552959530000123 ) ) ;
#12300 = CARTESIAN_POINT ( 'NONE',  ( 1.133692148650000009, 50.50000000000000000, -137.0552959530000123 ) ) ;
#12301 = EDGE_CURVE ( 'NONE', #16939, #5364, #4231, .T. ) ;
#12302 = LINE ( 'NONE', #5162, #21891 ) ;
#12303 = EDGE_CURVE ( 'NONE', #17345, #12071, #17529, .T. ) ;
#12304 = CYLINDRICAL_SURFACE ( 'NONE', #20042, 0.7500000000000016653 ) ;
#12305 = CONTEXT_DEPENDENT_SHAPE_REPRESENTATION ( #11909, #8197 ) ;
#12306 = CARTESIAN_POINT ( 'NONE',  ( 6.000000000160000013, 32.99305018889999275, -139.5552959529999839 ) ) ;
#12307 = DIRECTION ( 'NONE',  ( -2.257144641399999941E-12, 8.049635416090000264E-35, -1.000000000000000000 ) ) ;
#12308 = ORIENTED_EDGE ( 'NONE', *, *, #19990, .T. ) ;
#12309 = CARTESIAN_POINT ( 'NONE',  ( 25.96278831640000107, -46.03148680910000223, -136.0552959530000123 ) ) ;
#12310 = ORIENTED_EDGE ( 'NONE', *, *, #14112, .T. ) ;
#12311 = ORIENTED_EDGE ( 'NONE', *, *, #15053, .F. ) ;
#12312 = CARTESIAN_POINT ( 'NONE',  ( 4.500000000000000000, -3.500000000000000000, -140.0552959529999839 ) ) ;
#12313 = DIRECTION ( 'NONE',  ( 2.257144641399999941E-12, -4.009147065140000298E-51, 1.000000000000000000 ) ) ;
#12314 = DIRECTION ( 'NONE',  ( 4.430318231639999944E-12, -6.100259101500000139E-13, 1.000000000000000000 ) ) ;
#12315 = ORIENTED_EDGE ( 'NONE', *, *, #3948, .T. ) ;
#12316 = VECTOR ( 'NONE', #14907, 1000.000000000000000 ) ;
#12317 = CARTESIAN_POINT ( 'NONE',  ( -6.719401811558778803, 19.57621958799323636, -150.0552959530000123 ) ) ;
#12318 = CARTESIAN_POINT ( 'NONE',  ( 32.50000000000000000, 40.03620104880000241, -150.0552959529999839 ) ) ;
#12319 = CARTESIAN_POINT ( 'NONE',  ( -32.50000000000000000, 47.00000000000000000, -146.5552959529999839 ) ) ;
#12320 = DIRECTION ( 'NONE',  ( -1.000000000000000000, 0.000000000000000000, 2.257495777610000006E-12 ) ) ;
#12321 = CARTESIAN_POINT ( 'NONE',  ( -6.697834181631886707, 32.57753539646190433, -144.5849521621801443 ) ) ;
#12322 = EDGE_LOOP ( 'NONE', ( #14427, #18470, #19232, #3323, #19725 ) ) ;
#12323 = CARTESIAN_POINT ( 'NONE',  ( 9.797606456612053094, 36.24594602200216542, -141.6713346540966256 ) ) ;
#12324 = EDGE_CURVE ( 'NONE', #2980, #9295, #10513, .T. ) ;
#12325 = CARTESIAN_POINT ( 'NONE',  ( 6.500000000159999125, 20.50000000000000000, -139.5552959529999839 ) ) ;
#12326 = PLANE ( 'NONE',  #1149 ) ;
#12327 = ORIENTED_EDGE ( 'NONE', *, *, #7015, .T. ) ;
#12328 = FACE_OUTER_BOUND ( 'NONE', #15434, .T. ) ;
#12329 = VERTEX_POINT ( 'NONE', #10997 ) ;
#12330 = PLANE ( 'NONE',  #23114 ) ;
#12331 = DIRECTION ( 'NONE',  ( 1.000000000000000000, 0.000000000000000000, 2.257453483404482811E-12 ) ) ;
#12332 = EDGE_LOOP ( 'NONE', ( #1032, #19245, #5851, #15049 ) ) ;
#12333 = CARTESIAN_POINT ( 'NONE',  ( 8.157178495121881312, 38.46135633873473836, -146.0837389892857061 ) ) ;
#12334 = DIRECTION ( 'NONE',  ( -1.211690350419999855E-27, -2.765629237170000203E-27, 1.000000000000000000 ) ) ;
#12335 = EDGE_LOOP ( 'NONE', ( #3980, #14157, #22062, #9229 ) ) ;
#12336 = CARTESIAN_POINT ( 'NONE',  ( -15.36992937847549001, 41.12890580218349612, -146.3724425043323834 ) ) ;
#12337 = CARTESIAN_POINT ( 'NONE',  ( -4.510008323426233368, 42.75347665030082567, -150.0552959530000123 ) ) ;
#12338 = EDGE_LOOP ( 'NONE', ( #16292, #667, #12034 ) ) ;
#12339 = ORIENTED_EDGE ( 'NONE', *, *, #14375, .F. ) ;
#12340 = DIRECTION ( 'NONE',  ( -1.000000000000000000, 0.000000000000000000, 2.257495777610000006E-12 ) ) ;
#12341 = DIRECTION ( 'NONE',  ( -0.06298685227120542907, -0.9980143568310855251, 1.515824502950130739E-13 ) ) ;
#12342 = ORIENTED_EDGE ( 'NONE', *, *, #5613, .T. ) ;
#12343 = DIRECTION ( 'NONE',  ( 1.000000000000000000, 0.000000000000000000, 0.000000000000000000 ) ) ;
#12344 = ADVANCED_FACE ( 'NONE', ( #14584 ), #11217, .F. ) ;
#12345 = CARTESIAN_POINT ( 'NONE',  ( 12.94820732169999999, -17.45719265660000019, -147.5552959529999839 ) ) ;
#12346 = VERTEX_POINT ( 'NONE', #7204 ) ;
#12347 = CARTESIAN_POINT ( 'NONE',  ( -3.500000000000000000, 46.50000000000000000, -150.0552959529999839 ) ) ;
#12348 = VECTOR ( 'NONE', #619, 1000.000000000000000 ) ;
#12349 = EDGE_CURVE ( 'NONE', #19107, #22346, #12203, .T. ) ;
#12350 = ORIENTED_EDGE ( 'NONE', *, *, #8881, .F. ) ;
#12351 = DIRECTION ( 'NONE',  ( 0.000000000000000000, -1.000000000000000000, 0.000000000000000000 ) ) ;
#12352 = DIRECTION ( 'NONE',  ( -0.9913873220698726785, 0.1309625047069831461, -1.853446743629759619E-14 ) ) ;
#12353 =( REPRESENTATION_RELATIONSHIP ('NONE','NONE', #7672, #2821 ) REPRESENTATION_RELATIONSHIP_WITH_TRANSFORMATION ( #14575 )SHAPE_REPRESENTATION_RELATIONSHIP( ) );
#12354 = CARTESIAN_POINT ( 'NONE',  ( -14.60410653414054316, 40.19715529047051916, -145.9374667791834099 ) ) ;
#12355 = CARTESIAN_POINT ( 'NONE',  ( 6.477506801250000557, -13.91317765220000169, -146.5552959529999839 ) ) ;
#12356 = ORIENTED_EDGE ( 'NONE', *, *, #14647, .F. ) ;
#12357 = LINE ( 'NONE', #17851, #22652 ) ;
#12358 = EDGE_CURVE ( 'NONE', #6962, #20386, #4995, .T. ) ;
#12359 = CARTESIAN_POINT ( 'NONE',  ( -7.500000000000000000, 45.50000000000000000, -150.0552959529999839 ) ) ;
#12360 = CARTESIAN_POINT ( 'NONE',  ( -28.52142019844059107, 37.05975231236454448, -139.6605181376032476 ) ) ;
#12361 = DIRECTION ( 'NONE',  ( 0.000000000000000000, 1.000000000000000000, 0.000000000000000000 ) ) ;
#12362 = DIRECTION ( 'NONE',  ( 0.000000000000000000, 0.000000000000000000, 1.000000000000000000 ) ) ;
#12363 = VECTOR ( 'NONE', #13896, 1000.000000000000000 ) ;
#12364 = VECTOR ( 'NONE', #3046, 1000.000000000000000 ) ;
#12365 = ORIENTED_EDGE ( 'NONE', *, *, #12944, .F. ) ;
#12366 = CARTESIAN_POINT ( 'NONE',  ( 32.50000000000000000, 0.000000000000000000, -149.5552959529999839 ) ) ;
#12367 = DIRECTION ( 'NONE',  ( -1.000000000000000000, 0.000000000000000000, 0.000000000000000000 ) ) ;
#12368 = LINE ( 'NONE', #10460, #19745 ) ;
#12369 = CARTESIAN_POINT ( 'NONE',  ( -6.565507373470476082, 37.00519331014221081, -148.7410818962694066 ) ) ;
#12370 = DIRECTION ( 'NONE',  ( 1.000000000000000000, 0.000000000000000000, 2.516505522483685870E-12 ) ) ;
#12371 = CARTESIAN_POINT ( 'NONE',  ( -15.53720866509999965, -1.500000000000000000, -147.3052959529999839 ) ) ;
#12372 = VERTEX_POINT ( 'NONE', #186 ) ;
#12373 = ADVANCED_FACE ( 'NONE', ( #14341 ), #21852, .F. ) ;
#12374 = CARTESIAN_POINT ( 'NONE',  ( -9.334216945200001447, -17.19633444960000190, -145.5552959529999839 ) ) ;
#12375 = CARTESIAN_POINT ( 'NONE',  ( -12.28014746100000032, 36.97113097969999984, -148.4919582129999753 ) ) ;
#12376 = EDGE_CURVE ( 'NONE', #4637, #17721, #14467, .T. ) ;
#12377 = VERTEX_POINT ( 'NONE', #23389 ) ;
#12378 = B_SPLINE_CURVE_WITH_KNOTS ( 'NONE', 3,
 ( #12390, #15979, #12512, #19794, #10723, #21460, #14308, #7290, #5040, #18242, #21820, #23241, #3488, #1477, #18119, #3248, #14556, #19554, #10957, #8823, #18004, #5261, #9175, #158, #10481, #16451, #9046, #16100, #19666, #1715, #1954, #1830, #6935, #12280 ),
 .UNSPECIFIED., .F., .F.,
 ( 4, 2, 2, 2, 2, 2, 2, 2, 2, 2, 2, 2, 2, 2, 2, 2, 4 ),
 ( 0.000000000000000000, 0.06250000000000000000, 0.1250000000000000000, 0.1875000000000000000, 0.2500000000000000000, 0.3125000000000000000, 0.3750000000000000000, 0.4375000000000000000, 0.5000000000000000000, 0.5625000000000000000, 0.6250000000000000000, 0.6875000000000000000, 0.7500000000000000000, 0.8125000000000000000, 0.8750000000000000000, 0.9375000000000000000, 1.000000000000000000 ),
 .UNSPECIFIED. ) ;
#12379 = AXIS2_PLACEMENT_3D ( 'NONE', #18434, #20109, #3809 ) ;
#12380 = VECTOR ( 'NONE', #15623, 1000.000000000000000 ) ;
#12381 = DIRECTION ( 'NONE',  ( -2.256988247090000272E-12, 0.000000000000000000, -1.000000000000000000 ) ) ;
#12382 = ORIENTED_EDGE ( 'NONE', *, *, #21610, .F. ) ;
#12383 = CARTESIAN_POINT ( 'NONE',  ( -24.97797643630000053, 37.05442817780000553, -147.8575004449999994 ) ) ;
#12384 = CARTESIAN_POINT ( 'NONE',  ( 23.00000000000000000, 19.50000000000000000, -136.0552959530000123 ) ) ;
#12385 = CARTESIAN_POINT ( 'NONE',  ( 23.41308733940000053, -15.43505800149999985, -147.5552959529999839 ) ) ;
#12386 = CARTESIAN_POINT ( 'NONE',  ( 7.037218936158132543, 37.39203619355595976, -141.5783597022830236 ) ) ;
#12387 = EDGE_LOOP ( 'NONE', ( #22746, #5442 ) ) ;
#12388 = CARTESIAN_POINT ( 'NONE',  ( 4.554119375321583618, 27.76008370043824769, -150.0552959529999839 ) ) ;
#12389 = FACE_OUTER_BOUND ( 'NONE', #2233, .T. ) ;
#12390 = CARTESIAN_POINT ( 'NONE',  ( 4.750000000030000002, -35.98606797749999942, -136.0552959530000123 ) ) ;
#12391 = ORIENTED_EDGE ( 'NONE', *, *, #23052, .T. ) ;
#12392 = CARTESIAN_POINT ( 'NONE',  ( 18.66060904169178869, 20.09818317339687255, -136.0552959530421333 ) ) ;
#12393 = EDGE_CURVE ( 'NONE', #20527, #7013, #9314, .T. ) ;
#12394 = VERTEX_POINT ( 'NONE', #3753 ) ;
#12395 = VECTOR ( 'NONE', #6194, 1000.000000000000000 ) ;
#12396 = CARTESIAN_POINT ( 'NONE',  ( -6.599319970649999867, -19.98386714700000155, -146.5552959529999839 ) ) ;
#12397 = LINE ( 'NONE', #1482, #20606 ) ;
#12398 = CARTESIAN_POINT ( 'NONE',  ( 31.50000000000000000, -0.03620104880649999829, -137.0552959530000123 ) ) ;
#12399 = ORIENTED_EDGE ( 'NONE', *, *, #1119, .T. ) ;
#12400 = DIRECTION ( 'NONE',  ( 0.000000000000000000, 1.000000000000000000, 0.000000000000000000 ) ) ;
#12401 = DIRECTION ( 'NONE',  ( 0.9988198443106121038, -0.04856869991388110958, -1.110673412899570175E-14 ) ) ;
#12402 = EDGE_CURVE ( 'NONE', #14749, #4919, #18492, .T. ) ;
#12403 = ORIENTED_EDGE ( 'NONE', *, *, #14784, .T. ) ;
#12404 = CARTESIAN_POINT ( 'NONE',  ( 8.982728679470000088, -17.28848751049999777, -143.5552959529999839 ) ) ;
#12405 = CARTESIAN_POINT ( 'NONE',  ( 3.611688725869999975E-11, -33.03620104880000241, -136.0552959530000123 ) ) ;
#12406 = CARTESIAN_POINT ( 'NONE',  ( -15.78524365307784549, -40.07808196999505412, -150.0552959529999839 ) ) ;
#12407 = CARTESIAN_POINT ( 'NONE',  ( 5.148789539651774660, -45.97641955294970018, -136.0552959530116084 ) ) ;
#12408 = VECTOR ( 'NONE', #8928, 1000.000000000000000 ) ;
#12409 = CARTESIAN_POINT ( 'NONE',  ( -16.93971969060000049, -34.50000000000000000, -147.9894163970000136 ) ) ;
#12410 = ADVANCED_FACE ( 'NONE', ( #7428 ), #7086, .T. ) ;
#12411 = VECTOR ( 'NONE', #8254, 1000.000000000000000 ) ;
#12412 = CARTESIAN_POINT ( 'NONE',  ( -17.22605506639999717, 36.97564272059999979, -139.5994799229999899 ) ) ;
#12413 = CARTESIAN_POINT ( 'NONE',  ( 11.00000000010000001, 37.00000000000000000, -146.5552959529999839 ) ) ;
#12414 = CARTESIAN_POINT ( 'NONE',  ( -35.20609992760000040, 16.68710169819999933, -144.5552959529999839 ) ) ;
#12415 = LINE ( 'NONE', #9075, #20799 ) ;
#12416 = PRODUCT_DEFINITION_SHAPE ( 'NONE', 'NONE',  #20119 ) ;
#12417 = ORIENTED_EDGE ( 'NONE', *, *, #21475, .F. ) ;
#12418 = EDGE_LOOP ( 'NONE', ( #6646, #11948, #9555, #19327 ) ) ;
#12419 =( LENGTH_UNIT ( ) NAMED_UNIT ( * ) SI_UNIT ( .MILLI., .METRE. ) );
#12420 = EDGE_CURVE ( 'NONE', #14107, #23105, #9209, .T. ) ;
#12421 = ADVANCED_FACE ( 'NONE', ( #5763 ), #7196, .F. ) ;
#12422 = ORIENTED_EDGE ( 'NONE', *, *, #5333, .F. ) ;
#12423 = PLANE ( 'NONE',  #5340 ) ;
#12424 = CARTESIAN_POINT ( 'NONE',  ( -28.32042446336400232, 35.24116700710558092, -139.8750711406415235 ) ) ;
#12425 = ORIENTED_EDGE ( 'NONE', *, *, #20029, .F. ) ;
#12426 = LINE ( 'NONE', #8739, #15981 ) ;
#12427 = ADVANCED_FACE ( 'NONE', ( #2334 ), #9904, .T. ) ;
#12428 = AXIS2_PLACEMENT_3D ( 'NONE', #10748, #5526, #17459 ) ;
#12429 = ORIENTED_EDGE ( 'NONE', *, *, #11260, .T. ) ;
#12430 = CARTESIAN_POINT ( 'NONE',  ( -7.102348325422107145, 25.49999999999999645, -150.0552959530000123 ) ) ;
#12431 = EDGE_CURVE ( 'NONE', #20852, #21170, #4570, .T. ) ;
#12432 = CARTESIAN_POINT ( 'NONE',  ( -18.82091118356679971, 33.23810407333031947, -144.5979112941420226 ) ) ;
#12433 = PRESENTATION_LAYER_ASSIGNMENT (  '', '', ( #8996 ) ) ;
#12434 = CARTESIAN_POINT ( 'NONE',  ( -11.89394129276558232, 37.80475929424586923, -148.3421129316571125 ) ) ;
#12435 = LINE ( 'NONE', #10521, #4597 ) ;
#12436 = ORIENTED_EDGE ( 'NONE', *, *, #1474, .F. ) ;
#12437 = DIRECTION ( 'NONE',  ( 1.000000000000000000, 0.000000000000000000, 0.000000000000000000 ) ) ;
#12438 = VERTEX_POINT ( 'NONE', #13133 ) ;
#12439 = CARTESIAN_POINT ( 'NONE',  ( 9.120234899107126481, 35.63360340191769637, -141.9617131067784044 ) ) ;
#12440 = CARTESIAN_POINT ( 'NONE',  ( -7.500000000000000000, 45.50000000000000000, -151.0552959529999839 ) ) ;
#12441 = CARTESIAN_POINT ( 'NONE',  ( 11.68320006079999906, -20.50000000000000000, -148.5552959529999839 ) ) ;
#12442 = ORIENTED_EDGE ( 'NONE', *, *, #6044, .F. ) ;
#12443 = AXIS2_PLACEMENT_3D ( 'NONE', #19665, #3360, #7046 ) ;
#12444 = DIRECTION ( 'NONE',  ( 2.839308199620000013E-14, 3.568879590630000244E-13, 1.000000000000000000 ) ) ;
#12445 = CIRCLE ( 'NONE', #13971, 25.00000000000000000 ) ;
#12446 = ORIENTED_EDGE ( 'NONE', *, *, #18269, .T. ) ;
#12447 = ADVANCED_FACE ( 'NONE', ( #20404 ), #9613, .F. ) ;
#12448 = DIRECTION ( 'NONE',  ( 4.430233957459999899E-12, -6.110667527539999876E-13, 1.000000000000000000 ) ) ;
#12449 = CARTESIAN_POINT ( 'NONE',  ( -25.86630785129999666, -51.50000000000000000, -137.0552959530000123 ) ) ;
#12450 = B_SPLINE_CURVE_WITH_KNOTS ( 'NONE', 3,
 ( #12476, #1570, #16303, #19634, #8787, #16065, #18204, #23323, #7014, #3688, #10921, #9141, #16421, #1683, #14277, #21546, #5227, #4036 ),
 .UNSPECIFIED., .F., .F.,
 ( 4, 2, 2, 2, 2, 2, 2, 2, 4 ),
 ( 0.000000000000000000, 0.1250000000000000000, 0.2500000000000000000, 0.3750000000000000000, 0.5000000000000000000, 0.6250000000000000000, 0.7500000000000000000, 0.8750000000000000000, 1.000000000000000000 ),
 .UNSPECIFIED. ) ;
#12451 = ORIENTED_EDGE ( 'NONE', *, *, #21006, .T. ) ;
#12452 = CARTESIAN_POINT ( 'NONE',  ( -10.86836323999999898, 38.91206754959999614, -139.9811931129999891 ) ) ;
#12453 = EDGE_LOOP ( 'NONE', ( #2825, #22687, #1212, #13156, #649 ) ) ;
#12454 = CARTESIAN_POINT ( 'NONE',  ( -15.65026171697591018, 40.90570753890175837, -146.2089035856170369 ) ) ;
#12455 = ADVANCED_FACE ( 'NONE', ( #22050 ), #10843, .F. ) ;
#12456 = CARTESIAN_POINT ( 'NONE',  ( -29.25462571399999590, 37.92445966660000778, -140.5403777589999947 ) ) ;
#12457 = ORIENTED_EDGE ( 'NONE', *, *, #14028, .T. ) ;
#12458 =( NAMED_UNIT ( * ) PLANE_ANGLE_UNIT ( ) SI_UNIT ( $, .RADIAN. ) );
#12459 = ORIENTED_EDGE ( 'NONE', *, *, #18941, .T. ) ;
#12460 = CARTESIAN_POINT ( 'NONE',  ( -26.87389185232229138, 41.15523227550784924, -141.5790970697422892 ) ) ;
#12461 = LINE ( 'NONE', #23422, #10331 ) ;
#12462 = ORIENTED_EDGE ( 'NONE', *, *, #10380, .F. ) ;
#12463 = DIRECTION ( 'NONE',  ( -0.9954742291034677226, 0.09503188512734457583, 4.503697062742119365E-12 ) ) ;
#12464 = DIRECTION ( 'NONE',  ( 1.000000000000000000, 0.000000000000000000, -2.854859206178974232E-14 ) ) ;
#12465 = AXIS2_PLACEMENT_3D ( 'NONE', #13464, #8220, #2886 ) ;
#12466 = DIRECTION ( 'NONE',  ( -2.602084747549999882E-17, 1.000000000000000000, 5.873289694054760823E-29 ) ) ;
#12467 = ORIENTED_EDGE ( 'NONE', *, *, #5720, .T. ) ;
#12468 = PRESENTATION_LAYER_ASSIGNMENT (  '', '', ( #2228 ) ) ;
#12469 = DIRECTION ( 'NONE',  ( 0.000000000000000000, 0.000000000000000000, 1.000000000000000000 ) ) ;
#12470 = EDGE_LOOP ( 'NONE', ( #5102, #11862, #17850, #18148 ) ) ;
#12471 = PLANE ( 'NONE',  #1024 ) ;
#12472 = FACE_OUTER_BOUND ( 'NONE', #2599, .T. ) ;
#12473 = CARTESIAN_POINT ( 'NONE',  ( -13.46422577752552563, 37.93715959768575630, -139.9491268735157519 ) ) ;
#12474 = CARTESIAN_POINT ( 'NONE',  ( -28.65584425188693984, 38.23101052054714444, -139.6673458017931750 ) ) ;
#12475 = VERTEX_POINT ( 'NONE', #12872 ) ;
#12476 = CARTESIAN_POINT ( 'NONE',  ( 6.500000000040000003, 13.00000000000000000, -136.0552959530000123 ) ) ;
#12477 = DIRECTION ( 'NONE',  ( 0.000000000000000000, 0.000000000000000000, 1.000000000000000000 ) ) ;
#12478 = VECTOR ( 'NONE', #21888, 1000.000000000000000 ) ;
#12479 = LINE ( 'NONE', #14744, #19796 ) ;
#12480 = CARTESIAN_POINT ( 'NONE',  ( 31.50000000010000178, -40.03620104880000241, -137.0552959530000123 ) ) ;
#12481 = CARTESIAN_POINT ( 'NONE',  ( 27.68320006080000084, -32.50000000000000000, -150.0552959529999839 ) ) ;
#12482 = ADVANCED_FACE ( 'NONE', ( #14561 ), #12756, .F. ) ;
#12483 = CARTESIAN_POINT ( 'NONE',  ( -9.334216945200001447, -17.19633444960000190, -145.5552959529999839 ) ) ;
#12484 = VECTOR ( 'NONE', #20114, 1000.000000000000000 ) ;
#12485 = ORIENTED_EDGE ( 'NONE', *, *, #10093, .F. ) ;
#12486 = LINE ( 'NONE', #21553, #8413 ) ;
#12487 = CIRCLE ( 'NONE', #1117, 1.000000000000000888 ) ;
#12488 = DIRECTION ( 'NONE',  ( 2.507554887169999917E-12, 0.000000000000000000, -1.000000000000000000 ) ) ;
#12489 = VECTOR ( 'NONE', #13405, 1000.000000000000000 ) ;
#12490 = DIRECTION ( 'NONE',  ( 0.000000000000000000, 1.000000000000000000, 0.000000000000000000 ) ) ;
#12491 = DIRECTION ( 'NONE',  ( 0.000000000000000000, 0.000000000000000000, 1.000000000000000000 ) ) ;
#12492 = CARTESIAN_POINT ( 'NONE',  ( -8.309953467249998837, 35.25464643879999471, -140.3668538350000006 ) ) ;
#12493 = CARTESIAN_POINT ( 'NONE',  ( -15.00000000000000000, -43.00000000000000000, -136.0552959530000123 ) ) ;
#12494 = ORIENTED_EDGE ( 'NONE', *, *, #14460, .F. ) ;
#12495 = CARTESIAN_POINT ( 'NONE',  ( 16.25412235410000150, -22.59491385829999999, -146.5552959529999839 ) ) ;
#12496 = FACE_OUTER_BOUND ( 'NONE', #15440, .T. ) ;
#12497 = ORIENTED_EDGE ( 'NONE', *, *, #21266, .F. ) ;
#12498 = VECTOR ( 'NONE', #4266, 999.9999999999998863 ) ;
#12499 = VECTOR ( 'NONE', #918, 1000.000000000000000 ) ;
#12500 = DIRECTION ( 'NONE',  ( -3.994014902950000436E-29, 1.000000000000000000, -4.148443855749999753E-27 ) ) ;
#12501 = ORIENTED_EDGE ( 'NONE', *, *, #22570, .F. ) ;
#12502 = VECTOR ( 'NONE', #20001, 1000.000000000000000 ) ;
#12503 = CARTESIAN_POINT ( 'NONE',  ( -23.81040386161897260, 37.71789450755535711, -147.9004385756058753 ) ) ;
#12504 = CARTESIAN_POINT ( 'NONE',  ( -29.47785954729999958, 39.65718555499999809, -141.4786507110000287 ) ) ;
#12505 = VECTOR ( 'NONE', #4264, 1000.000000000000000 ) ;
#12506 = LINE ( 'NONE', #1708, #12408 ) ;
#12507 = CARTESIAN_POINT ( 'NONE',  ( 7.498126930446614935, 38.11651284494442393, -141.8183173536806692 ) ) ;
#12508 = ORIENTED_EDGE ( 'NONE', *, *, #12736, .T. ) ;
#12509 = CARTESIAN_POINT ( 'NONE',  ( -11.56119896032659256, 36.14006801961227922, -140.1188298284611449 ) ) ;
#12510 = CARTESIAN_POINT ( 'NONE',  ( -18.64329452426891365, 32.49620444683537102, -144.6932856329320884 ) ) ;
#12511 = CARTESIAN_POINT ( 'NONE',  ( -9.105481712864866850, 39.02735606833573456, -146.8299818849519340 ) ) ;
#12512 = CARTESIAN_POINT ( 'NONE',  ( 4.332174032671896491, -35.55157851246247702, -136.0552959530098178 ) ) ;
#12513 = EDGE_CURVE ( 'NONE', #9187, #4619, #3493, .T. ) ;
#12514 = ORIENTED_EDGE ( 'NONE', *, *, #1419, .T. ) ;
#12515 = ADVANCED_FACE ( 'NONE', ( #10607 ), #16563, .F. ) ;
#12516 = DIRECTION ( 'NONE',  ( 0.000000000000000000, 1.000000000000000000, 0.000000000000000000 ) ) ;
#12517 = CIRCLE ( 'NONE', #11365, 35.00000000000000000 ) ;
#12518 = AXIS2_PLACEMENT_3D ( 'NONE', #5608, #13332, #11071 ) ;
#12519 = ORIENTED_EDGE ( 'NONE', *, *, #1379, .F. ) ;
#12520 = CARTESIAN_POINT ( 'NONE',  ( -9.334216945200001447, -17.19633444960000190, -146.5552959529999839 ) ) ;
#12521 = DIRECTION ( 'NONE',  ( 4.430318231639999944E-12, -6.100259101500000139E-13, 1.000000000000000000 ) ) ;
#12522 = CARTESIAN_POINT ( 'NONE',  ( -6.719401811520419265, 19.57621958799322570, -136.0552959529848351 ) ) ;
#12523 = ORIENTED_EDGE ( 'NONE', *, *, #20595, .F. ) ;
#12524 = CIRCLE ( 'NONE', #1531, 2.000000000000000000 ) ;
#12525 = CARTESIAN_POINT ( 'NONE',  ( 18.95053822279999878, -50.99999999949999818, -150.0552959529999839 ) ) ;
#12526 = DIRECTION ( 'NONE',  ( 0.1146332952500066227, 0.9934078757590583120, 9.947598300640582187E-14 ) ) ;
#12527 = ORIENTED_EDGE ( 'NONE', *, *, #19537, .F. ) ;
#12528 = CARTESIAN_POINT ( 'NONE',  ( -15.00000000000000000, -43.00000000000000000, -136.0552959530000123 ) ) ;
#12529 = CARTESIAN_POINT ( 'NONE',  ( 3.611688725869999975E-11, -21.03620104879999886, -136.0552959530000123 ) ) ;
#12530 = CYLINDRICAL_SURFACE ( 'NONE', #11231, 2.000000000000002220 ) ;
#12531 = CARTESIAN_POINT ( 'NONE',  ( -32.50000000000000000, -17.50000000000000000, -151.0552959529999839 ) ) ;
#12532 = FACE_OUTER_BOUND ( 'NONE', #22073, .T. ) ;
#12533 = CARTESIAN_POINT ( 'NONE',  ( -25.80099178304864793, 37.02638091262011955, -140.6905788942592608 ) ) ;
#12534 = SHAPE_DEFINITION_REPRESENTATION ( #7390, #23186 ) ;
#12535 = FACE_OUTER_BOUND ( 'NONE', #19215, .T. ) ;
#12536 = AXIS2_PLACEMENT_3D ( 'NONE', #6353, #22905, #6590 ) ;
#12537 = CARTESIAN_POINT ( 'NONE',  ( 15.50000000000000000, 39.50000000000000000, -137.0552959530000123 ) ) ;
#12538 = VECTOR ( 'NONE', #5770, 1000.000000000000000 ) ;
#12539 = PLANE ( 'NONE',  #12824 ) ;
#12540 = CIRCLE ( 'NONE', #2313, 3.000000000000000000 ) ;
#12541 = ORIENTED_EDGE ( 'NONE', *, *, #7034, .T. ) ;
#12542 = UNCERTAINTY_MEASURE_WITH_UNIT (LENGTH_MEASURE( 1.000000000000000082E-05 ), #8176, 'distance_accuracy_value', 'NONE');
#12543 = ORIENTED_EDGE ( 'NONE', *, *, #6474, .T. ) ;
#12544 = ORIENTED_EDGE ( 'NONE', *, *, #3569, .F. ) ;
#12545 = CARTESIAN_POINT ( 'NONE',  ( -16.36776575232984143, 35.42538575923208555, -147.6161688091087569 ) ) ;
#12546 = CARTESIAN_POINT ( 'NONE',  ( -13.20713333982466509, 36.31039189040361492, -147.8273893801373902 ) ) ;
#12547 = CARTESIAN_POINT ( 'NONE',  ( -34.50000000000000000, -35.00000000000000000, -140.0552959529999839 ) ) ;
#12548 = LINE ( 'NONE', #7324, #18379 ) ;
#12549 = EDGE_LOOP ( 'NONE', ( #4005, #6993, #7685, #5347 ) ) ;
#12550 = DIRECTION ( 'NONE',  ( 0.000000000000000000, 0.000000000000000000, 1.000000000000000000 ) ) ;
#12551 = ADVANCED_FACE ( 'NONE', ( #19913 ), #20031, .T. ) ;
#12552 = CARTESIAN_POINT ( 'NONE',  ( -20.00879305376257022, 35.51518944883265760, -140.9236936935650135 ) ) ;
#12553 = LINE ( 'NONE', #8976, #9965 ) ;
#12554 = CARTESIAN_POINT ( 'NONE',  ( -30.49999999990000177, 47.50000000000000000, -140.5552959529999839 ) ) ;
#12555 = AXIS2_PLACEMENT_3D ( 'NONE', #2503, #20583, #7488 ) ;
#12556 = ORIENTED_EDGE ( 'NONE', *, *, #6506, .F. ) ;
#12557 = VECTOR ( 'NONE', #6241, 1000.000000000000000 ) ;
#12558 = CARTESIAN_POINT ( 'NONE',  ( 3.385736135899999992E-11, -2.273736754430000208E-12, -137.0552959530000123 ) ) ;
#12559 = ORIENTED_EDGE ( 'NONE', *, *, #6340, .F. ) ;
#12560 = CARTESIAN_POINT ( 'NONE',  ( 8.891181416159669837, 35.55106431351824625, -142.0179551233528343 ) ) ;
#12561 = ADVANCED_FACE ( 'NONE', ( #17891 ), #3613, .T. ) ;
#12562 = DIRECTION ( 'NONE',  ( 0.6459422414661292189, -0.7633862853691524286, 2.257144641400451094E-12 ) ) ;
#12563 = ADVANCED_FACE ( 'NONE', ( #1609 ), #21937, .T. ) ;
#12564 = DIRECTION ( 'NONE',  ( 0.1000233216789610108, 0.9949850929136109245, -3.588240815588595806E-13 ) ) ;
#12565 = EDGE_LOOP ( 'NONE', ( #17227, #22539, #11320, #7292 ) ) ;
#12566 = EDGE_CURVE ( 'NONE', #3293, #3797, #18011, .T. ) ;
#12567 = ADVANCED_FACE ( 'NONE', ( #10963, #11082 ), #8829, .T. ) ;
#12568 = DIRECTION ( 'NONE',  ( 2.257171095940000041E-12, 1.003664318210000046E-28, 1.000000000000000000 ) ) ;
#12569 = ORIENTED_EDGE ( 'NONE', *, *, #21321, .F. ) ;
#12570 = CARTESIAN_POINT ( 'NONE',  ( 12.01554901919999985, -37.47280209340000567, -144.5552959529999839 ) ) ;
#12571 = VECTOR ( 'NONE', #20419, 1000.000000000000000 ) ;
#12572 = CARTESIAN_POINT ( 'NONE',  ( -4.499999999969999109, 40.00000000000000000, -137.0552959530000123 ) ) ;
#12573 = AXIS2_PLACEMENT_3D ( 'NONE', #13580, #17395, #8342 ) ;
#12574 = VERTEX_POINT ( 'NONE', #9052 ) ;
#12575 = CARTESIAN_POINT ( 'NONE',  ( -11.42599417689999974, 41.52668172479999953, -143.7505393120000292 ) ) ;
#12576 = ORIENTED_EDGE ( 'NONE', *, *, #6041, .F. ) ;
#12577 = CARTESIAN_POINT ( 'NONE',  ( -10.00000000000000000, 25.50000000000000000, -150.0552959529999839 ) ) ;
#12578 = LINE ( 'NONE', #14609, #6410 ) ;
#12579 = ORIENTED_EDGE ( 'NONE', *, *, #10136, .F. ) ;
#12580 = DIRECTION ( 'NONE',  ( 1.000000000000000000, 0.000000000000000000, 0.000000000000000000 ) ) ;
#12581 = B_SPLINE_CURVE_WITH_KNOTS ( 'NONE', 1,
 ( #22456, #6266 ),
 .UNSPECIFIED., .F., .F.,
 ( 2, 2 ),
 ( -12.63369214860000156, 6.000000000000000000 ),
 .UNSPECIFIED. ) ;
#12582 = EDGE_LOOP ( 'NONE', ( #12523, #5971, #17134, #4250 ) ) ;
#12583 = CARTESIAN_POINT ( 'NONE',  ( -26.11358249223754413, 38.93857572900594022, -139.6801797896497703 ) ) ;
#12584 = ADVANCED_FACE ( 'NONE', ( #16109 ), #1958, .F. ) ;
#12585 = CARTESIAN_POINT ( 'NONE',  ( 1.133692148650000009, -50.50000000000000000, -136.5552959530000123 ) ) ;
#12586 = EDGE_LOOP ( 'NONE', ( #11968, #5991, #15135, #21141 ) ) ;
#12587 = DIRECTION ( 'NONE',  ( 0.000000000000000000, 0.000000000000000000, 1.000000000000000000 ) ) ;
#12588 = ADVANCED_FACE ( 'NONE', ( #162 ), #7296, .F. ) ;
#12589 = LINE ( 'NONE', #20091, #22054 ) ;
#12590 = DIRECTION ( 'NONE',  ( -0.9892101392001055871, 0.1465035852930155202, 0.000000000000000000 ) ) ;
#12591 = EDGE_LOOP ( 'NONE', ( #2051, #10294, #13827, #6443 ) ) ;
#12592 = CARTESIAN_POINT ( 'NONE',  ( 12.50000000010000001, 24.10555127549999810, -143.5552959529999839 ) ) ;
#12593 = AXIS2_PLACEMENT_3D ( 'NONE', #18709, #18357, #5615 ) ;
#12594 = VECTOR ( 'NONE', #13370, 1000.000000000000000 ) ;
#12595 = VECTOR ( 'NONE', #20581, 1000.000000000000000 ) ;
#12596 = EDGE_CURVE ( 'NONE', #5244, #4587, #8943, .T. ) ;
#12597 = EDGE_CURVE ( 'NONE', #11102, #10168, #21710, .T. ) ;
#12598 = ORIENTED_EDGE ( 'NONE', *, *, #17365, .F. ) ;
#12599 = DIRECTION ( 'NONE',  ( -0.9919007982877544594, 0.1270149847699686418, 4.766005912188822159E-14 ) ) ;
#12600 = EDGE_CURVE ( 'NONE', #12006, #20679, #7664, .T. ) ;
#12601 = DIRECTION ( 'NONE',  ( -1.000000000000000000, -3.717264591378872697E-16, 0.000000000000000000 ) ) ;
#12602 = CARTESIAN_POINT ( 'NONE',  ( -16.86519360499094233, 39.73476227100517377, -140.3032793073522555 ) ) ;
#12603 = CARTESIAN_POINT ( 'NONE',  ( -32.50000000000000000, 21.50000000000000000, -150.5552959529999839 ) ) ;
#12604 = EDGE_LOOP ( 'NONE', ( #9690, #5129, #20517, #11987 ) ) ;
#12605 = LINE ( 'NONE', #19879, #16568 ) ;
#12606 = DIRECTION ( 'NONE',  ( -1.000000000000000000, 0.000000000000000000, 0.000000000000000000 ) ) ;
#12607 = FACE_OUTER_BOUND ( 'NONE', #17561, .T. ) ;
#12608 = CARTESIAN_POINT ( 'NONE',  ( -18.07392865170000107, -18.00000000000000000, -146.3157682190000060 ) ) ;
#12609 = LINE ( 'NONE', #14400, #4509 ) ;
#12610 = VECTOR ( 'NONE', #20934, 1000.000000000000000 ) ;
#12611 = ORIENTED_EDGE ( 'NONE', *, *, #8513, .T. ) ;
#12612 = VECTOR ( 'NONE', #8122, 1000.000000000000000 ) ;
#12613 = AXIS2_PLACEMENT_3D ( 'NONE', #5240, #12491, #23449 ) ;
#12614 = CARTESIAN_POINT ( 'NONE',  ( 11.00000000000000000, 37.00000000000000000, -149.5552959529999839 ) ) ;
#12615 = CARTESIAN_POINT ( 'NONE',  ( 8.750000000000000000, -40.23606797749999942, -150.0552959529999839 ) ) ;
#12616 = FACE_BOUND ( 'NONE', #1109, .T. ) ;
#12617 = CARTESIAN_POINT ( 'NONE',  ( -6.288682382039059604, 41.28368337079415085, -144.4167712528175969 ) ) ;
#12618 = CARTESIAN_POINT ( 'NONE',  ( -13.68932041746861294, -43.75542847055635320, -136.0552959530029682 ) ) ;
#12619 = VERTEX_POINT ( 'NONE', #2647 ) ;
#12620 = CARTESIAN_POINT ( 'NONE',  ( -27.48801997220000004, 39.21796412529999998, -147.0196846460000017 ) ) ;
#12621 = DIRECTION ( 'NONE',  ( 0.7633862853691524286, -0.6459422414661292189, 2.187565684170436280E-17 ) ) ;
#12622 = EDGE_LOOP ( 'NONE', ( #6390, #7798, #9272, #15138 ) ) ;
#12623 = ADVANCED_FACE ( 'NONE', ( #4418 ), #9533, .T. ) ;
#12624 = EDGE_CURVE ( 'NONE', #6697, #11089, #15132, .T. ) ;
#12625 = COLOUR_RGB ( '', 0.09019608, 0.27058824, 0.51372549) ;
#12626 = CYLINDRICAL_SURFACE ( 'NONE', #10216, 2.500000000000000444 ) ;
#12627 = ORIENTED_EDGE ( 'NONE', *, *, #3909, .T. ) ;
#12628 = AXIS2_PLACEMENT_3D ( 'NONE', #8647, #9002, #12702 ) ;
#12629 = CARTESIAN_POINT ( 'NONE',  ( -23.82650726623105086, 39.03244537584987484, -146.9745935326799895 ) ) ;
#12630 = CARTESIAN_POINT ( 'NONE',  ( -30.24492469408960105, 40.76033517006445805, -142.6215232399929960 ) ) ;
#12631 = DIRECTION ( 'NONE',  ( -0.9896415801065049367, 0.1435602414469282218, 8.993136838065500309E-12 ) ) ;
#12632 = CARTESIAN_POINT ( 'NONE',  ( 7.668714288586619077, 38.24858600746667037, -141.8894180608807574 ) ) ;
#12633 = ORIENTED_EDGE ( 'NONE', *, *, #20027, .F. ) ;
#12634 = CARTESIAN_POINT ( 'NONE',  ( -10.74201573257056630, 32.87128505482456120, -141.4462505804974057 ) ) ;
#12635 = CARTESIAN_POINT ( 'NONE',  ( -19.59223779464246817, 34.04810666035614730, -140.2228890206432652 ) ) ;
#12636 = CARTESIAN_POINT ( 'NONE',  ( -8.971913342289999704, 37.83624783359999810, -148.2794752869999968 ) ) ;
#12637 = DIRECTION ( 'NONE',  ( -2.507771768023035002E-12, -1.592654560756634986E-17, 1.000000000000000000 ) ) ;
#12638 = ORIENTED_EDGE ( 'NONE', *, *, #21730, .F. ) ;
#12639 = CARTESIAN_POINT ( 'NONE',  ( 17.57650987483295069, 23.28094649262697402, -136.0552959530396606 ) ) ;
#12640 = FILL_AREA_STYLE ('',( #3609 ) ) ;
#12641 = ORIENTED_EDGE ( 'NONE', *, *, #8433, .F. ) ;
#12642 = CARTESIAN_POINT ( 'NONE',  ( -8.462973826026347623, 36.94736262684725858, -140.5165674475847766 ) ) ;
#12643 = CARTESIAN_POINT ( 'NONE',  ( -23.86695901000000219, 38.68196870779999585, -148.0474502900000005 ) ) ;
#12644 = CARTESIAN_POINT ( 'NONE',  ( 16.61718498210000305, -18.75502267109999721, -142.5552959529999839 ) ) ;
#12645 = AXIS2_PLACEMENT_3D ( 'NONE', #1458, #11908, #987 ) ;
#12646 = EDGE_LOOP ( 'NONE', ( #13414, #13391, #3496 ) ) ;
#12647 = FACE_OUTER_BOUND ( 'NONE', #21967, .T. ) ;
#12648 = CARTESIAN_POINT ( 'NONE',  ( 18.18320006080000084, -6.500000000000000000, -148.5552959529999839 ) ) ;
#12649 = ORIENTED_EDGE ( 'NONE', *, *, #21107, .F. ) ;
#12650 = ADVANCED_FACE ( 'NONE', ( #4195 ), #2182, .F. ) ;
#12651 = PLANE ( 'NONE',  #12170 ) ;
#12652 = EDGE_CURVE ( 'NONE', #3632, #16967, #15370, .T. ) ;
#12653 = CARTESIAN_POINT ( 'NONE',  ( 17.88103053855265401, 20.98519100495539291, -150.0552959529999839 ) ) ;
#12654 = CARTESIAN_POINT ( 'NONE',  ( -13.50000000000000355, -43.19908942272522268, -150.0552959529999839 ) ) ;
#12655 = EDGE_CURVE ( 'NONE', #7237, #12619, #6580, .T. ) ;
#12656 = CARTESIAN_POINT ( 'NONE',  ( -23.51619327739999932, 36.94101002280000046, -140.1031831869999849 ) ) ;
#12657 = FACE_OUTER_BOUND ( 'NONE', #22676, .T. ) ;
#12658 = CARTESIAN_POINT ( 'NONE',  ( 3.611688725869999975E-11, 32.96379895120000469, -136.0552959530000123 ) ) ;
#12659 = APPLICATION_PROTOCOL_DEFINITION ( 'draft international standard', 'automotive_design', 1998, #15264 ) ;
#12660 = CYLINDRICAL_SURFACE ( 'NONE', #16223, 0.4999999999999936717 ) ;
#12661 = VERTEX_POINT ( 'NONE', #17436 ) ;
#12662 = DIRECTION ( 'NONE',  ( 0.000000000000000000, 1.000000000000000000, 0.000000000000000000 ) ) ;
#12663 = DIRECTION ( 'NONE',  ( 1.000000000000000000, 0.000000000000000000, -4.429789868254374596E-12 ) ) ;
#12664 = ORIENTED_EDGE ( 'NONE', *, *, #20248, .F. ) ;
#12665 = VERTEX_POINT ( 'NONE', #15258 ) ;
#12666 = SURFACE_STYLE_USAGE ( .BOTH. , #20290 ) ;
#12667 = ORIENTED_EDGE ( 'NONE', *, *, #17606, .T. ) ;
#12668 = CARTESIAN_POINT ( 'NONE',  ( -15.57039528521051963, 36.22627288621195873, -147.5570433397655847 ) ) ;
#12669 = CARTESIAN_POINT ( 'NONE',  ( -13.39436545728456451, 34.84914659774037204, -147.2640033608687702 ) ) ;
#12670 = VERTEX_POINT ( 'NONE', #20267 ) ;
#12671 = ADVANCED_FACE ( 'NONE', ( #16681 ), #5848, .T. ) ;
#12672 = CARTESIAN_POINT ( 'NONE',  ( 6.992624432290238445, 28.00000000000003553, -136.0552959530157864 ) ) ;
#12673 = ORIENTED_EDGE ( 'NONE', *, *, #22202, .T. ) ;
#12674 = CARTESIAN_POINT ( 'NONE',  ( 2.508811538190000245, -14.35090895149999923, -145.5552959529999839 ) ) ;
#12675 = DIRECTION ( 'NONE',  ( 0.000000000000000000, 0.000000000000000000, 1.000000000000000000 ) ) ;
#12676 = CARTESIAN_POINT ( 'NONE',  ( -12.02450515625771210, 36.94061592734458088, -147.5849826166100627 ) ) ;
#12677 = DIRECTION ( 'NONE',  ( 0.000000000000000000, 1.000000000000000000, 0.000000000000000000 ) ) ;
#12678 = EDGE_LOOP ( 'NONE', ( #5091, #6351, #14070, #22361 ) ) ;
#12679 = CARTESIAN_POINT ( 'NONE',  ( 12.50000000010902745, 16.89444872450000190, -139.5552959530157864 ) ) ;
#12680 = ORIENTED_EDGE ( 'NONE', *, *, #4173, .F. ) ;
#12681 = CARTESIAN_POINT ( 'NONE',  ( 9.522541048056565316, 35.90250400897288330, -141.8090149961586803 ) ) ;
#12682 = ADVANCED_FACE ( 'NONE', ( #2530 ), #5968, .T. ) ;
#12683 =( BOUNDED_SURFACE ( )  B_SPLINE_SURFACE ( 5, 5, ( 
 ( #3452, #10685, #17966, #1679, #19873, #3568 ),
 ( #11946, #1155, #2142, #19214, #22123, #2379 ),
 ( #7589, #22469, #22006, #22348, #4146, #15086 ),
 ( #18428, #16634, #469, #10156, #5692, #4705 ),
 ( #7706, #20451, #14863, #9480, #17428, #11154 ),
 ( #8388, #16756, #21013, #3921, #22233, #18775 ),
 ( #13750, #15214, #2924, #20567, #9599, #11383 ),
 ( #9709, #6045, #5809, #582, #18666, #12951 ),
 ( #16873, #9362, #20228, #7818, #347, #14972 ),
 ( #13177, #13066, #13296, #4268, #20338, #4031 ),
 ( #11498, #2488, #11265, #18538, #2256, #16985 ),
 ( #699, #7931, #6491, #5923, #23029, #8847 ) ),
 .UNSPECIFIED., .F., .F., .F. ) 
 B_SPLINE_SURFACE_WITH_KNOTS ( ( 6, 3, 3, 6 ),
 ( 6, 6 ),
 ( 0.000000000000000000, 4.398006073320000375, 8.633600727160001043, 12.71824907600000110 ),
 ( 1.570796326630355066, 3.141592653590000062 ),
 .UNSPECIFIED. ) 
 GEOMETRIC_REPRESENTATION_ITEM ( )  RATIONAL_B_SPLINE_SURFACE ( (
 ( 0.2500000000000000000, 0.2499999999790369909, 0.2999999999685555307, 0.3999999999580740040, 0.5999999999580739596, 1.000000000000000000),
 ( 0.2500000000000000000, 0.2499999999790369909, 0.2999999999685555307, 0.3999999999580740040, 0.5999999999580739596, 1.000000000000000000),
 ( 0.2500000000000000000, 0.2499999999790369909, 0.2999999999685555307, 0.3999999999580740040, 0.5999999999580739596, 1.000000000000000000),
 ( 0.2500000000000000000, 0.2499999999790369909, 0.2999999999685555307, 0.3999999999580740040, 0.5999999999580739596, 1.000000000000000000),
 ( 0.2500000000000000000, 0.2499999999790369909, 0.2999999999685555307, 0.3999999999580740040, 0.5999999999580739596, 1.000000000000000000),
 ( 0.2500000000000000000, 0.2499999999790369909, 0.2999999999685555307, 0.3999999999580740040, 0.5999999999580739596, 1.000000000000000000),
 ( 0.2500000000000000000, 0.2499999999790369909, 0.2999999999685555307, 0.3999999999580740040, 0.5999999999580739596, 1.000000000000000000),
 ( 0.2500000000000000000, 0.2499999999790369909, 0.2999999999685555307, 0.3999999999580740040, 0.5999999999580739596, 1.000000000000000000),
 ( 0.2500000000000000000, 0.2499999999790369909, 0.2999999999685555307, 0.3999999999580740040, 0.5999999999580739596, 1.000000000000000000),
 ( 0.2500000000000000000, 0.2499999999790369909, 0.2999999999685555307, 0.3999999999580740040, 0.5999999999580739596, 1.000000000000000000),
 ( 0.2500000000000000000, 0.2499999999790369909, 0.2999999999685555307, 0.3999999999580740040, 0.5999999999580739596, 1.000000000000000000),
 ( 0.2500000000000000000, 0.2499999999790369909, 0.2999999999685555307, 0.3999999999580740040, 0.5999999999580739596, 1.000000000000000000) ) ) 
 REPRESENTATION_ITEM ( '' )  SURFACE ( )  );
#12684 = CARTESIAN_POINT ( 'NONE',  ( 22.50000000000000000, 36.50000000000000000, -137.0552959530000123 ) ) ;
#12685 = DIRECTION ( 'NONE',  ( -1.000000000000000000, 0.000000000000000000, 2.257144641399999941E-12 ) ) ;
#12686 = VERTEX_POINT ( 'NONE', #13105 ) ;
#12687 = ADVANCED_FACE ( 'NONE', ( #2307 ), #16803, .F. ) ;
#12688 = DIRECTION ( 'NONE',  ( 1.000000000000000000, 0.000000000000000000, 0.000000000000000000 ) ) ;
#12689 = ORIENTED_EDGE ( 'NONE', *, *, #11313, .F. ) ;
#12690 = CARTESIAN_POINT ( 'NONE',  ( -19.10036853996236772, 37.06903765908678849, -148.2030617969735715 ) ) ;
#12691 = FACE_BOUND ( 'NONE', #16946, .T. ) ;
#12692 = ORIENTED_EDGE ( 'NONE', *, *, #16680, .T. ) ;
#12693 = CARTESIAN_POINT ( 'NONE',  ( -26.68542098469999857, 39.18140699330000132, -140.9632721460000084 ) ) ;
#12694 = ORIENTED_EDGE ( 'NONE', *, *, #3709, .F. ) ;
#12695 = VECTOR ( 'NONE', #17539, 1000.000000000000000 ) ;
#12696 = CARTESIAN_POINT ( 'NONE',  ( -15.76067864000701668, 37.76810578663741325, -147.5051738567275379 ) ) ;
#12697 = CARTESIAN_POINT ( 'NONE',  ( 0.5000000001659999915, 24.10555127549999810, -136.5552959530000123 ) ) ;
#12698 = ORIENTED_EDGE ( 'NONE', *, *, #770, .T. ) ;
#12699 = EDGE_CURVE ( 'NONE', #4966, #21958, #20986, .T. ) ;
#12700 = EDGE_LOOP ( 'NONE', ( #23180, #13394, #12879, #754 ) ) ;
#12701 = CARTESIAN_POINT ( 'NONE',  ( -26.71657219920165005, 37.82487237221160825, -139.7343082328227410 ) ) ;
#12702 = DIRECTION ( 'NONE',  ( -2.257144641399999941E-12, 0.000000000000000000, -1.000000000000000000 ) ) ;
#12703 = ORIENTED_EDGE ( 'NONE', *, *, #1878, .T. ) ;
#12704 = DIRECTION ( 'NONE',  ( -0.9949850929136110356, 0.1000233216789610385, -5.551115123125783491E-15 ) ) ;
#12705 = CARTESIAN_POINT ( 'NONE',  ( -10.92974397189781222, 35.65249901646877362, -140.8582538894084735 ) ) ;
#12706 = DIRECTION ( 'NONE',  ( -2.507771768019999718E-12, 0.000000000000000000, 1.000000000000000000 ) ) ;
#12707 = VERTEX_POINT ( 'NONE', #7748 ) ;
#12708 = LINE ( 'NONE', #20097, #2631 ) ;
#12709 = EDGE_CURVE ( 'NONE', #8241, #22607, #13220, .T. ) ;
#12710 = DIRECTION ( 'NONE',  ( -1.000000000000000000, 5.094701932209999624E-24, 2.257144641399999941E-12 ) ) ;
#12711 = ORIENTED_EDGE ( 'NONE', *, *, #22479, .F. ) ;
#12712 = LINE ( 'NONE', #6891, #20787 ) ;
#12713 = DIRECTION ( 'NONE',  ( -2.602084747549999882E-17, 1.000000000000000000, 5.873289694040000105E-29 ) ) ;
#12714 = ADVANCED_FACE ( 'NONE', ( #7978 ), #22515, .F. ) ;
#12715 = CARTESIAN_POINT ( 'NONE',  ( -17.45987344088444360, 41.16328378089777829, -141.5750803238402398 ) ) ;
#12716 = DIRECTION ( 'NONE',  ( 1.000000000000000000, 0.000000000000000000, -2.257120985840000117E-12 ) ) ;
#12717 = ORIENTED_EDGE ( 'NONE', *, *, #195, .T. ) ;
#12718 = CARTESIAN_POINT ( 'NONE',  ( -34.47299999999999898, 14.00000000000000000, -144.0552959529999839 ) ) ;
#12719 = CARTESIAN_POINT ( 'NONE',  ( -25.64792992860000354, 37.04465132570000208, -139.7265440090000084 ) ) ;
#12720 = DIRECTION ( 'NONE',  ( 1.000000000000000000, 0.000000000000000000, -4.430318231639999944E-12 ) ) ;
#12721 = CARTESIAN_POINT ( 'NONE',  ( 1.500000000000000000, -3.500000000000000000, -140.0552959529999839 ) ) ;
#12722 = LINE ( 'NONE', #3222, #12968 ) ;
#12723 = CARTESIAN_POINT ( 'NONE',  ( 26.50000000000000000, -20.50000000000000000, -143.5552959529999839 ) ) ;
#12724 = ORIENTED_EDGE ( 'NONE', *, *, #13398, .F. ) ;
#12725 = DIRECTION ( 'NONE',  ( -4.430233957459999899E-12, 6.092903959140000514E-13, -1.000000000000000000 ) ) ;
#12726 = EDGE_CURVE ( 'NONE', #6969, #21917, #3961, .T. ) ;
#12727 = CARTESIAN_POINT ( 'NONE',  ( -13.50000000000000000, -43.00000000000000000, -136.0552959530000123 ) ) ;
#12728 = CARTESIAN_POINT ( 'NONE',  ( 3.714756346922168273, -6.421918030004948541, -150.0552959529999839 ) ) ;
#12729 = EDGE_CURVE ( 'NONE', #3746, #2000, #10112, .T. ) ;
#12730 = VECTOR ( 'NONE', #4999, 1000.000000000000000 ) ;
#12731 = CARTESIAN_POINT ( 'NONE',  ( -5.664837119873038951, 39.54185838768819394, -147.6076384376017927 ) ) ;
#12732 = FACE_OUTER_BOUND ( 'NONE', #11482, .T. ) ;
#12733 = EDGE_CURVE ( 'NONE', #22524, #8477, #2768, .T. ) ;
#12734 = VERTEX_POINT ( 'NONE', #14056 ) ;
#12735 = LINE ( 'NONE', #7149, #11712 ) ;
#12736 = EDGE_CURVE ( 'NONE', #21645, #9692, #12260, .T. ) ;
#12737 = AXIS2_PLACEMENT_3D ( 'NONE', #1644, #16143, #8865 ) ;
#12738 = CARTESIAN_POINT ( 'NONE',  ( 13.13369214870000157, 51.00000000000000000, -137.0552959530000123 ) ) ;
#12739 = ORIENTED_EDGE ( 'NONE', *, *, #12267, .F. ) ;
#12740 = PLANE ( 'NONE',  #6052 ) ;
#12741 = ORIENTED_EDGE ( 'NONE', *, *, #7758, .F. ) ;
#12742 = CARTESIAN_POINT ( 'NONE',  ( -23.91604154053268161, 38.38020865605560772, -147.3412701355220520 ) ) ;
#12743 = DIRECTION ( 'NONE',  ( 1.377713942929999840E-10, 1.000000000000000000, 0.000000000000000000 ) ) ;
#12744 = CARTESIAN_POINT ( 'NONE',  ( -12.50000000000000000, 42.50000000000000000, -136.0552959530000123 ) ) ;
#12745 = CARTESIAN_POINT ( 'NONE',  ( 7.511313393277872841, 38.12817115245120192, -141.8241438720509962 ) ) ;
#12746 = ORIENTED_EDGE ( 'NONE', *, *, #5698, .F. ) ;
#12747 = CARTESIAN_POINT ( 'NONE',  ( -11.16897700298565077, 36.05264020273449432, -139.4334584778495412 ) ) ;
#12748 = CIRCLE ( 'NONE', #13117, 3.000000000000000000 ) ;
#12749 = CARTESIAN_POINT ( 'NONE',  ( -19.54668701385130447, 37.05673630843254784, -139.5622637237151196 ) ) ;
#12750 = PLANE ( 'NONE',  #1075 ) ;
#12751 = CARTESIAN_POINT ( 'NONE',  ( 13.68320006080000084, -21.50000000000000000, -143.5552959529999839 ) ) ;
#12752 = DIRECTION ( 'NONE',  ( 1.000000000000000000, -5.094701932209999624E-24, 0.000000000000000000 ) ) ;
#12753 = ORIENTED_EDGE ( 'NONE', *, *, #6201, .T. ) ;
#12754 = CARTESIAN_POINT ( 'NONE',  ( 19.59648046430000079, 50.76338628540000286, -149.5552959529999839 ) ) ;
#12755 = EDGE_CURVE ( 'NONE', #16477, #598, #14509, .T. ) ;
#12756 = PLANE ( 'NONE',  #3503 ) ;
#12757 = LINE ( 'NONE', #14205, #8024 ) ;
#12758 = DIRECTION ( 'NONE',  ( 0.000000000000000000, 0.000000000000000000, 1.000000000000000000 ) ) ;
#12759 = ORIENTED_EDGE ( 'NONE', *, *, #387, .T. ) ;
#12760 = CARTESIAN_POINT ( 'NONE',  ( -5.733381482170000432, 39.34803470290000149, -147.3316303149999840 ) ) ;
#12761 = DIRECTION ( 'NONE',  ( 2.257171095940000041E-12, -7.494005416210000121E-16, 1.000000000000000000 ) ) ;
#12762 = AXIS2_PLACEMENT_3D ( 'NONE', #9018, #21547, #23440 ) ;
#12763 = VECTOR ( 'NONE', #23491, 1000.000000000000000 ) ;
#12764 = ORIENTED_EDGE ( 'NONE', *, *, #20551, .F. ) ;
#12765 = CARTESIAN_POINT ( 'NONE',  ( -6.327504759656895850, -17.27997690994742896, -145.5552959530004671 ) ) ;
#12766 = DIRECTION ( 'NONE',  ( 1.000000000000000000, 0.000000000000000000, 0.000000000000000000 ) ) ;
#12767 = DIRECTION ( 'NONE',  ( 0.000000000000000000, 1.000000000000000000, 0.000000000000000000 ) ) ;
#12768 = B_SPLINE_CURVE_WITH_KNOTS ( 'NONE', 3,
 ( #5574, #12825, #20098, #2137, #11039, #9251, #16521, #230, #22000, #5689, #20923, #4726, #6512, #11495, #6386, #11970, #11728, #13647, #20795, #17218, #4489, #13293, #8279, #4612, #2718, #11611, #932, #20562, #695, #18772, #2827, #16981, #8158, #6159, #9706, #10182, #19009, #2947, #9947, #15432, #15324, #7926 ),
 .UNSPECIFIED., .F., .F.,
 ( 4, 2, 2, 2, 2, 2, 2, 2, 2, 2, 2, 2, 2, 2, 2, 2, 2, 2, 2, 2, 4 ),
 ( 0.000000000000000000, 0.06249999999999189537, 0.09374999999998742672, 0.1093749999999862887, 0.1249999999999851508, 0.1874999999999937272, 0.2500000000000023315, 0.3125000000000108802, 0.3437500000000158762, 0.3750000000000208722, 0.5000000000000379696, 0.5625000000000442979, 0.5937500000000451861, 0.6250000000000461853, 0.6875000000000444089, 0.7500000000000426326, 0.8125000000000408562, 0.8437500000000387468, 0.8593750000000348610, 0.8750000000000309752, 1.000000000000000000 ),
 .UNSPECIFIED. ) ;
#12769 = CARTESIAN_POINT ( 'NONE',  ( -25.09512484594771209, 36.12507003254601301, -148.5419237647928981 ) ) ;
#12770 = DIRECTION ( 'NONE',  ( -0.06298685227120542907, -0.9980143568310855251, 1.534772309240130738E-13 ) ) ;
#12771 = CARTESIAN_POINT ( 'NONE',  ( -9.434278515689999978, -18.41834002140000237, -147.5552959529999839 ) ) ;
#12772 = CONTEXT_DEPENDENT_SHAPE_REPRESENTATION ( #12353, #1009 ) ;
#12773 = DIRECTION ( 'NONE',  ( 0.000000000000000000, 0.000000000000000000, 1.000000000000000000 ) ) ;
#12774 = PLANE ( 'NONE',  #21889 ) ;
#12775 = CARTESIAN_POINT ( 'NONE',  ( 17.44013884619999999, -20.67371738400000325, -144.5552959529999839 ) ) ;
#12776 = EDGE_LOOP ( 'NONE', ( #18638, #14531, #23474, #12067 ) ) ;
#12777 = AXIS2_PLACEMENT_3D ( 'NONE', #21835, #8840, #3507 ) ;
#12778 = UNCERTAINTY_MEASURE_WITH_UNIT (LENGTH_MEASURE( 1.000000000000000082E-05 ), #1720, 'distance_accuracy_value', 'NONE');
#12779 = ORIENTED_EDGE ( 'NONE', *, *, #13398, .T. ) ;
#12780 = SURFACE_SIDE_STYLE ('',( #420 ) ) ;
#12781 = ADVANCED_FACE ( 'NONE', ( #4663 ), #5016, .F. ) ;
#12782 = ORIENTED_EDGE ( 'NONE', *, *, #8881, .T. ) ;
#12783 = CARTESIAN_POINT ( 'NONE',  ( -16.33553080621575404, 33.80379307428399471, -145.7770475876280329 ) ) ;
#12784 = DIRECTION ( 'NONE',  ( 0.000000000000000000, 0.000000000000000000, -1.000000000000000000 ) ) ;
#12785 = DIRECTION ( 'NONE',  ( 0.000000000000000000, 2.259525899719999991E-12, 1.000000000000000000 ) ) ;
#12786 = CARTESIAN_POINT ( 'NONE',  ( 11.07581004124147483, 26.46257514628838692, -136.0552959530250234 ) ) ;
#12787 = VERTEX_POINT ( 'NONE', #15833 ) ;
#12788 = DIRECTION ( 'NONE',  ( 1.000000000000000000, 0.000000000000000000, 0.000000000000000000 ) ) ;
#12789 = CARTESIAN_POINT ( 'NONE',  ( -19.57725164000000007, 32.58775676329999271, -144.7853266960000269 ) ) ;
#12790 = DIRECTION ( 'NONE',  ( 0.000000000000000000, 1.000000000000000000, 0.000000000000000000 ) ) ;
#12791 = VERTEX_POINT ( 'NONE', #13932 ) ;
#12792 = LINE ( 'NONE', #14700, #15222 ) ;
#12793 = ORIENTED_EDGE ( 'NONE', *, *, #1834, .F. ) ;
#12794 = CARTESIAN_POINT ( 'NONE',  ( 9.336697666959173247, 35.75503528090352745, -141.8873347153283930 ) ) ;
#12795 = VECTOR ( 'NONE', #17722, 1000.000000000000000 ) ;
#12796 = CARTESIAN_POINT ( 'NONE',  ( 4.500000000000000000, -3.500000000000000000, -140.0552959529999839 ) ) ;
#12797 = CARTESIAN_POINT ( 'NONE',  ( -33.50000000000000000, 76.00000000000000000, -132.5552959530000123 ) ) ;
#12798 = ORIENTED_EDGE ( 'NONE', *, *, #10962, .F. ) ;
#12799 = CARTESIAN_POINT ( 'NONE',  ( 8.750000000000000000, -39.23606797749999942, -150.0552959529999839 ) ) ;
#12800 = ORIENTED_EDGE ( 'NONE', *, *, #13969, .T. ) ;
#12801 = CARTESIAN_POINT ( 'NONE',  ( 4.800813058665234223, -47.52045733082537993, -150.0552959530000123 ) ) ;
#12802 = CARTESIAN_POINT ( 'NONE',  ( 27.18320006080000084, 3.500000000000000000, -148.5552959529999839 ) ) ;
#12804 = VERTEX_POINT ( 'NONE', #22871 ) ;
#12803 = AXIS2_PLACEMENT_3D ( 'NONE', #1974, #10982, #22291 ) ;
#12805 = CARTESIAN_POINT ( 'NONE',  ( -26.27746988921043680, 37.69287412588059993, -140.6313975853602756 ) ) ;
#12806 = EDGE_LOOP ( 'NONE', ( #3549, #727, #12627, #16729, #22227 ) ) ;
#12807 = EDGE_CURVE ( 'NONE', #2580, #361, #11902, .T. ) ;
#12808 = CARTESIAN_POINT ( 'NONE',  ( -21.53618355987887867, 33.35162261426351904, -146.0341402268610125 ) ) ;
#12809 = MECHANICAL_DESIGN_GEOMETRIC_PRESENTATION_REPRESENTATION (  '', ( #18141 ), #4461 ) ;
#12810 = FACE_OUTER_BOUND ( 'NONE', #23297, .T. ) ;
#12811 = EDGE_CURVE ( 'NONE', #15840, #22265, #4777, .T. ) ;
#12812 = ORIENTED_EDGE ( 'NONE', *, *, #8504, .T. ) ;
#12813 = DIRECTION ( 'NONE',  ( 0.000000000000000000, 0.000000000000000000, 1.000000000000000000 ) ) ;
#12814 = ORIENTED_EDGE ( 'NONE', *, *, #5311, .F. ) ;
#12815 = CARTESIAN_POINT ( 'NONE',  ( 31.50000000000000000, -40.03620104870000063, -136.0552959530000123 ) ) ;
#12816 =( REPRESENTATION_RELATIONSHIP ('NONE','NONE', #7672, #17559 ) REPRESENTATION_RELATIONSHIP_WITH_TRANSFORMATION ( #20394 )SHAPE_REPRESENTATION_RELATIONSHIP( ) );
#12817 = CARTESIAN_POINT ( 'NONE',  ( 16.25766103973663945, -22.55971267323774399, -145.5552959530246540 ) ) ;
#12818 = DIRECTION ( 'NONE',  ( 1.211690350419999855E-27, 2.765629237170000203E-27, -1.000000000000000000 ) ) ;
#12819 =( BOUNDED_CURVE ( )  B_SPLINE_CURVE ( 5, ( #11809, #15861, #18012, #12288, #5147, #3494, #21711, #8705, #19801, #12643, #6941, #3614 ),
 .UNSPECIFIED., .F., .F. ) 
 B_SPLINE_CURVE_WITH_KNOTS ( ( 6, 3, 3, 6 ),
 ( 0.000000000000000000, 4.509114667229999540, 8.972055907920001516, 13.39149027789999913 ),
 .UNSPECIFIED. ) 
 CURVE ( )  GEOMETRIC_REPRESENTATION_ITEM ( )  RATIONAL_B_SPLINE_CURVE ( ( 0.2500000000000000000, 0.2500000000000000000, 0.2500000000000000000, 0.2500000000000000000, 0.2500000000000000000, 0.2500000000000000000, 0.2500000000000000000, 0.2500000000000000000, 0.2500000000000000000, 0.2500000000000000000, 0.2500000000000000000, 0.2500000000000000000 ) ) 
 REPRESENTATION_ITEM ( '' )  );
#12820 = CARTESIAN_POINT ( 'NONE',  ( 32.00000000000000000, 39.80430157320000006, -149.5552959529999839 ) ) ;
#12821 = CARTESIAN_POINT ( 'NONE',  ( -18.35824191589999899, -34.50000000000000000, -144.8157682190000060 ) ) ;
#12822 = ORIENTED_EDGE ( 'NONE', *, *, #4924, .F. ) ;
#12823 = CARTESIAN_POINT ( 'NONE',  ( -14.01657753870000001, 36.22806874879999839, -140.5479840249999768 ) ) ;
#12824 = AXIS2_PLACEMENT_3D ( 'NONE', #3515, #1053, #18146 ) ;
#12825 = CARTESIAN_POINT ( 'NONE',  ( 8.599236905806820985, 35.50003553908390330, -146.0553226073559756 ) ) ;
#12826 = CONICAL_SURFACE ( 'NONE', #5981, 2.000000000000003553, 0.7853981633970000820 ) ;
#12827 = VERTEX_POINT ( 'NONE', #1228 ) ;
#12828 = CARTESIAN_POINT ( 'NONE',  ( 3.190307906134843829, -4.257167980435450083, -150.0552959529999271 ) ) ;
#12829 = EDGE_CURVE ( 'NONE', #567, #19467, #10699, .T. ) ;
#12830 = CARTESIAN_POINT ( 'NONE',  ( -21.16045305574322200, -4.749999999999998224, -146.3157682190070830 ) ) ;
#12831 = CARTESIAN_POINT ( 'NONE',  ( -17.08670351461686820, 41.11123597602360746, -141.6546470616082161 ) ) ;
#12832 = CARTESIAN_POINT ( 'NONE',  ( -29.47785954729999958, 39.65718555499999809, -141.4786507110000287 ) ) ;
#12833 = EDGE_LOOP ( 'NONE', ( #11402, #22726, #14512, #493 ) ) ;
#12834 = FACE_BOUND ( 'NONE', #18673, .T. ) ;
#12835 = CARTESIAN_POINT ( 'NONE',  ( -30.49999999990000177, 46.25000000000000000, -140.5552959529999839 ) ) ;
#12836 = CARTESIAN_POINT ( 'NONE',  ( -17.75130813170000366, 41.00325609940000504, -141.6328284839999867 ) ) ;
#12837 = LINE ( 'NONE', #12723, #16293 ) ;
#12838 = EDGE_CURVE ( 'NONE', #12998, #5773, #16413, .T. ) ;
#12839 = ORIENTED_EDGE ( 'NONE', *, *, #11859, .T. ) ;
#12840 = CARTESIAN_POINT ( 'NONE',  ( -27.40802390352900630, 34.81902089894730778, -146.9145522347566839 ) ) ;
#12841 = VECTOR ( 'NONE', #14808, 1000.000000000000000 ) ;
#12842 = DIRECTION ( 'NONE',  ( 1.000000000000000000, 0.000000000000000000, 0.000000000000000000 ) ) ;
#12843 = CARTESIAN_POINT ( 'NONE',  ( 4.892699081698736130, -6.500000000000000000, -150.0552959529999839 ) ) ;
#12844 = VECTOR ( 'NONE', #11477, 1000.000000000000000 ) ;
#12845 = CARTESIAN_POINT ( 'NONE',  ( -6.732165765376294075, 38.94235323983919272, -148.2714551560809753 ) ) ;
#12846 = DIRECTION ( 'NONE',  ( 0.000000000000000000, 1.000000000000000000, 0.000000000000000000 ) ) ;
#12847 = ORIENTED_EDGE ( 'NONE', *, *, #19990, .F. ) ;
#12848 = CARTESIAN_POINT ( 'NONE',  ( 2.068499633510000102, -14.99362786250000035, -148.0552959529999839 ) ) ;
#12849 = EDGE_CURVE ( 'NONE', #6393, #712, #1619, .T. ) ;
#12850 = DIRECTION ( 'NONE',  ( 0.000000000000000000, 1.000000000000000000, 0.000000000000000000 ) ) ;
#12851 = ORIENTED_EDGE ( 'NONE', *, *, #11557, .T. ) ;
#12852 = EDGE_LOOP ( 'NONE', ( #11290, #9847, #87, #3967, #9563, #5375, #22417 ) ) ;
#12853 = CARTESIAN_POINT ( 'NONE',  ( 5.961949895415374456, -3.109416060109817970, -136.0552959530134842 ) ) ;
#12854 = CIRCLE ( 'NONE', #23500, 0.5000000000000004441 ) ;
#12855 = EDGE_CURVE ( 'NONE', #15273, #8129, #3002, .T. ) ;
#12856 = VECTOR ( 'NONE', #20556, 1000.000000000000000 ) ;
#12857 = CARTESIAN_POINT ( 'NONE',  ( -31.00000000000000000, -50.00000000000000000, -149.5552959529999839 ) ) ;
#12858 = EDGE_CURVE ( 'NONE', #4598, #14014, #8025, .T. ) ;
#12859 = AXIS2_PLACEMENT_3D ( 'NONE', #15098, #709, #11276 ) ;
#12860 = DIRECTION ( 'NONE',  ( 3.994014902950000436E-29, -1.000000000000000000, 4.148443855749999753E-27 ) ) ;
#12861 = CARTESIAN_POINT ( 'NONE',  ( -3.500000000000000000, 34.00000000000000000, -150.0552959529999839 ) ) ;
#12862 = VERTEX_POINT ( 'NONE', #3121 ) ;
#12863 =( NAMED_UNIT ( * ) SI_UNIT ( $, .STERADIAN. ) SOLID_ANGLE_UNIT ( ) );
#12864 = CARTESIAN_POINT ( 'NONE',  ( -19.57725164000000007, 32.58775676329999271, -144.7853266960000269 ) ) ;
#12865 = ADVANCED_FACE ( 'NONE', ( #17627 ), #16922, .F. ) ;
#12866 = CARTESIAN_POINT ( 'NONE',  ( 25.18320006080000084, -34.50000000000000000, -148.5552959529999839 ) ) ;
#12867 = DIRECTION ( 'NONE',  ( 2.257144641399999941E-12, -4.009147065140000298E-51, 1.000000000000000000 ) ) ;
#12868 = VECTOR ( 'NONE', #19150, 1000.000000000000000 ) ;
#12869 = EDGE_CURVE ( 'NONE', #16889, #7959, #9562, .T. ) ;
#12870 = DIRECTION ( 'NONE',  ( 2.257144641399999941E-12, -4.009147065140000298E-51, 1.000000000000000000 ) ) ;
#12871 = DIRECTION ( 'NONE',  ( -0.7633862853691523176, 0.6459422414661291079, 0.000000000000000000 ) ) ;
#12872 = CARTESIAN_POINT ( 'NONE',  ( -8.916553640509999212, -11.88594259849999979, -143.5552959529999839 ) ) ;
#12873 = CARTESIAN_POINT ( 'NONE',  ( 32.50000000000000000, -21.03620104879999886, -137.0552959530000123 ) ) ;
#12874 = CARTESIAN_POINT ( 'NONE',  ( 2.508811538200000246, -14.35090895149999923, -144.5552959529999839 ) ) ;
#12875 = VECTOR ( 'NONE', #226, 1000.000000000000000 ) ;
#12876 = ORIENTED_EDGE ( 'NONE', *, *, #14483, .F. ) ;
#12877 = CARTESIAN_POINT ( 'NONE',  ( -6.981168498894938956, 37.84839353770540527, -147.7381749008708312 ) ) ;
#12878 = CIRCLE ( 'NONE', #22381, 9.000000000000000000 ) ;
#12879 = ORIENTED_EDGE ( 'NONE', *, *, #21562, .T. ) ;
#12880 = LINE ( 'NONE', #281, #1585 ) ;
#12881 = AXIS2_PLACEMENT_3D ( 'NONE', #13456, #20722, #4416 ) ;
#12882 = AXIS2_PLACEMENT_3D ( 'NONE', #17933, #1650, #23403 ) ;
#12883 = FACE_OUTER_BOUND ( 'NONE', #22215, .T. ) ;
#12884 = CARTESIAN_POINT ( 'NONE',  ( 19.91945158500000090, 51.14507942810000429, -149.5552959529999839 ) ) ;
#12885 = CARTESIAN_POINT ( 'NONE',  ( 4.999999999879999990, -3.000000000000000000, -135.2552959529999725 ) ) ;
#12886 = CARTESIAN_POINT ( 'NONE',  ( -12.28014746100000032, 36.97113097969999984, -148.4919582129999753 ) ) ;
#12887 = ADVANCED_FACE ( 'NONE', ( #19773 ), #11283, .F. ) ;
#12888 = B_SPLINE_CURVE_WITH_KNOTS ( 'NONE', 3,
 ( #17784, #13864, #10286, #23264, #21373, #6956, #19337, #3385, #7076, #14221 ),
 .UNSPECIFIED., .F., .F.,
 ( 4, 2, 2, 2, 4 ),
 ( 0.000000000000000000, 0.2500000000000000555, 0.5000000000000001110, 0.7500000000000000000, 1.000000000000000000 ),
 .UNSPECIFIED. ) ;
#12889 = LINE ( 'NONE', #14803, #8184 ) ;
#12890 = EDGE_CURVE ( 'NONE', #11235, #896, #13196, .T. ) ;
#12891 = DIRECTION ( 'NONE',  ( -1.000000000000000000, 0.000000000000000000, 2.257120985840000117E-12 ) ) ;
#12892 = CARTESIAN_POINT ( 'NONE',  ( -15.00000000000000000, -44.50000000000000000, -137.0552959530000123 ) ) ;
#12893 = FACE_OUTER_BOUND ( 'NONE', #22184, .T. ) ;
#12894 = AXIS2_PLACEMENT_3D ( 'NONE', #3475, #10712, #10252 ) ;
#12895 = CARTESIAN_POINT ( 'NONE',  ( -32.50000000000000000, -18.00000000000000000, -151.0552959529999839 ) ) ;
#12896 = CIRCLE ( 'NONE', #5679, 0.5000000000000004441 ) ;
#12897 = EDGE_LOOP ( 'NONE', ( #3009, #14276, #4216 ) ) ;
#12898 = VECTOR ( 'NONE', #190, 1000.000000000000000 ) ;
#12899 = ORIENTED_EDGE ( 'NONE', *, *, #16396, .T. ) ;
#12900 = VECTOR ( 'NONE', #10741, 1000.000000000000000 ) ;
#12901 = ORIENTED_EDGE ( 'NONE', *, *, #12376, .F. ) ;
#12902 = CARTESIAN_POINT ( 'NONE',  ( -13.18072986969131932, 37.07863008620352474, -148.2345011165226651 ) ) ;
#12903 = DIRECTION ( 'NONE',  ( -1.000000000000000000, 0.000000000000000000, 1.701177084980000217E-20 ) ) ;
#12904 = LINE ( 'NONE', #14692, #3945 ) ;
#12905 = ORIENTED_EDGE ( 'NONE', *, *, #5874, .T. ) ;
#12906 = FACE_OUTER_BOUND ( 'NONE', #5901, .T. ) ;
#12907 = CARTESIAN_POINT ( 'NONE',  ( -20.10082943595380911, 33.21594955552029660, -142.1386041078769154 ) ) ;
#12908 = DIRECTION ( 'NONE',  ( 0.000000000000000000, 1.000000000000000000, 0.000000000000000000 ) ) ;
#12909 = ORIENTED_EDGE ( 'NONE', *, *, #17667, .T. ) ;
#12910 = CARTESIAN_POINT ( 'NONE',  ( -20.54812748657687038, 36.93719815735425271, -140.4704715740689949 ) ) ;
#12911 = CARTESIAN_POINT ( 'NONE',  ( 9.790782907733147411, 37.76485605363462383, -141.6749984784336505 ) ) ;
#12912 = VECTOR ( 'NONE', #19636, 1000.000000000000227 ) ;
#12913 = CIRCLE ( 'NONE', #18631, 15.00000000000000178 ) ;
#12914 = EDGE_CURVE ( 'NONE', #2213, #7225, #22488, .T. ) ;
#12915 = DIRECTION ( 'NONE',  ( 1.000000000000000000, 0.000000000000000000, -2.257453483404485639E-12 ) ) ;
#12916 = AXIS2_PLACEMENT_3D ( 'NONE', #13509, #13872, #18995 ) ;
#12917 = AXIS2_PLACEMENT_3D ( 'NONE', #17957, #10673, #23425 ) ;
#12918 = ADVANCED_FACE ( 'NONE', ( #16655 ), #11518, .F. ) ;
#12919 = CARTESIAN_POINT ( 'NONE',  ( -24.06602356369428009, 36.94557182216776425, -148.2530914611035939 ) ) ;
#12920 = ORIENTED_EDGE ( 'NONE', *, *, #1695, .T. ) ;
#12921 = DIRECTION ( 'NONE',  ( 1.000000000000000000, 2.602084704489999637E-17, -1.701177084980000217E-20 ) ) ;
#12922 = ORIENTED_EDGE ( 'NONE', *, *, #17106, .F. ) ;
#12923 =( NAMED_UNIT ( * ) PLANE_ANGLE_UNIT ( ) SI_UNIT ( $, .RADIAN. ) );
#12924 = ORIENTED_EDGE ( 'NONE', *, *, #8382, .F. ) ;
#12925 = CARTESIAN_POINT ( 'NONE',  ( -25.68538705770549058, 39.50692289490424258, -140.7105351162441877 ) ) ;
#12926 = ORIENTED_EDGE ( 'NONE', *, *, #13143, .T. ) ;
#12927 = CARTESIAN_POINT ( 'NONE',  ( -22.81311670109966272, 32.52853389434195464, -143.5568795629989722 ) ) ;
#12928 = EDGE_LOOP ( 'NONE', ( #21110, #816, #19270, #22563 ) ) ;
#12929 = CARTESIAN_POINT ( 'NONE',  ( -29.82391180389999619, 40.55477172079999804, -144.2881336360000262 ) ) ;
#12930 = ORIENTED_EDGE ( 'NONE', *, *, #15852, .T. ) ;
#12931 = APPLICATION_PROTOCOL_DEFINITION ( 'draft international standard', 'automotive_design', 1998, #23319 ) ;
#12932 = CONICAL_SURFACE ( 'NONE', #11783, 1.499999999999999334, 0.9827937232469998730 ) ;
#12933 = VECTOR ( 'NONE', #4965, 1000.000000000000000 ) ;
#12934 = ORIENTED_EDGE ( 'NONE', *, *, #9178, .T. ) ;
#12935 = LINE ( 'NONE', #7574, #16326 ) ;
#12936 = CARTESIAN_POINT ( 'NONE',  ( -7.506111428109999650, 33.37436714639999735, -146.3147224710000387 ) ) ;
#12937 = CARTESIAN_POINT ( 'NONE',  ( 11.07581004119133539, 26.46257514629612118, -150.0552959530000123 ) ) ;
#12938 = CARTESIAN_POINT ( 'NONE',  ( -6.547730170590000398, -18.66441632429999942, -148.5552959529999839 ) ) ;
#12939 = CARTESIAN_POINT ( 'NONE',  ( -10.13972653286922565, 34.91672950339960835, -140.8637739126610313 ) ) ;
#12940 = DIRECTION ( 'NONE',  ( 0.000000000000000000, 0.000000000000000000, 1.000000000000000000 ) ) ;
#12941 = VERTEX_POINT ( 'NONE', #9728 ) ;
#12942 = CYLINDRICAL_SURFACE ( 'NONE', #1505, 1.500000000000000444 ) ;
#12943 = EDGE_CURVE ( 'NONE', #8645, #3037, #3117, .T. ) ;
#12944 = EDGE_CURVE ( 'NONE', #903, #17493, #16774, .T. ) ;
#12945 = FACE_OUTER_BOUND ( 'NONE', #7455, .T. ) ;
#12946 = EDGE_CURVE ( 'NONE', #19545, #8311, #9618, .T. ) ;
#12947 = VECTOR ( 'NONE', #4850, 1000.000000000000000 ) ;
#12948 = VERTEX_POINT ( 'NONE', #20471 ) ;
#12949 = AXIS2_PLACEMENT_3D ( 'NONE', #21352, #1131, #8362 ) ;
#12950 = LINE ( 'NONE', #19982, #17350 ) ;
#12951 = CARTESIAN_POINT ( 'NONE',  ( -11.76172848620000089, 40.95326072219999958, -146.5101368410000191 ) ) ;
#12952 = CARTESIAN_POINT ( 'NONE',  ( -17.43685409200564251, 41.68787803771047606, -144.5118622863669202 ) ) ;
#12953 = CARTESIAN_POINT ( 'NONE',  ( 1.357896944619999990, -19.89221232270000073, -148.5552959529999839 ) ) ;
#12954 = ORIENTED_EDGE ( 'NONE', *, *, #3277, .F. ) ;
#12955 = FILL_AREA_STYLE_COLOUR ( '', #14734 ) ;
#12956 = LINE ( 'NONE', #21669, #23031 ) ;
#12957 = CARTESIAN_POINT ( 'NONE',  ( -33.50000000000000000, -1.000000000000000000, -151.0552959529999839 ) ) ;
#12958 = LINE ( 'NONE', #9263, #6451 ) ;
#12959 = DIRECTION ( 'NONE',  ( -0.09606172499277226828, -0.9953753789357124848, 8.268133652477615271E-13 ) ) ;
#12960 = CARTESIAN_POINT ( 'NONE',  ( -5.500000000000000000, 44.50000000000000000, -150.0552959529999839 ) ) ;
#12961 = CARTESIAN_POINT ( 'NONE',  ( -20.09055976259235266, 41.19265711152617371, -141.7594002370568944 ) ) ;
#12962 = ORIENTED_EDGE ( 'NONE', *, *, #3555, .F. ) ;
#12963 =( BOUNDED_SURFACE ( )  B_SPLINE_SURFACE ( 5, 5, ( 
 ( #6377, #4604, #15543, #1170, #21264, #8400 ),
 ( #11843, #2818, #6616, #12081, #19355, #10049 ),
 ( #22809, #6505, #13770, #21030, #10174, #19227 ),
 ( #15673, #7328, #10878, #5304, #18282, #8742 ),
 ( #14696, #3401, #3529, #5182, #18157, #20061 ),
 ( #12432, #16020, #1870, #1996, #16485, #12789 ),
 ( #5651, #14589, #11002, #3644, #20188, #9092 ),
 ( #191, #14473, #6972, #8862, #12907, #3759 ),
 ( #14237, #21857, #84, #23282, #16378, #5541 ),
 ( #9215, #19707, #12552, #7434, #21965, #16141 ),
 ( #3883, #14348, #11117, #23395, #18389, #21501 ),
 ( #10642, #17925, #1641, #7091, #18042, #19943 ) ),
 .UNSPECIFIED., .F., .F., .F. ) 
 B_SPLINE_SURFACE_WITH_KNOTS ( ( 6, 3, 3, 6 ),
 ( 6, 6 ),
 ( 0.000000000000000000, 4.059123295939999210, 8.340116530639999581, 12.86134770560000007 ),
 ( 1.570796326526080033, 3.141592653590000062 ),
 .UNSPECIFIED. ) 
 GEOMETRIC_REPRESENTATION_ITEM ( )  RATIONAL_B_SPLINE_SURFACE ( (
 ( 0.2500000000000000000, 0.2499999999657600003, 0.2999999999486395175, 0.3999999999315194676, 0.5999999999315199783, 1.000000000000000000),
 ( 0.2500000000000000000, 0.2499999999657600003, 0.2999999999486395175, 0.3999999999315194676, 0.5999999999315199783, 1.000000000000000000),
 ( 0.2500000000000000000, 0.2499999999657600003, 0.2999999999486395175, 0.3999999999315194676, 0.5999999999315199783, 1.000000000000000000),
 ( 0.2500000000000000000, 0.2499999999657600003, 0.2999999999486395175, 0.3999999999315194676, 0.5999999999315199783, 1.000000000000000000),
 ( 0.2500000000000000000, 0.2499999999657600003, 0.2999999999486395175, 0.3999999999315194676, 0.5999999999315199783, 1.000000000000000000),
 ( 0.2500000000000000000, 0.2499999999657600003, 0.2999999999486395175, 0.3999999999315194676, 0.5999999999315199783, 1.000000000000000000),
 ( 0.2500000000000000000, 0.2499999999657600003, 0.2999999999486395175, 0.3999999999315194676, 0.5999999999315199783, 1.000000000000000000),
 ( 0.2500000000000000000, 0.2499999999657600003, 0.2999999999486395175, 0.3999999999315194676, 0.5999999999315199783, 1.000000000000000000),
 ( 0.2500000000000000000, 0.2499999999657600003, 0.2999999999486395175, 0.3999999999315194676, 0.5999999999315199783, 1.000000000000000000),
 ( 0.2500000000000000000, 0.2499999999657600003, 0.2999999999486395175, 0.3999999999315194676, 0.5999999999315199783, 1.000000000000000000),
 ( 0.2500000000000000000, 0.2499999999657600003, 0.2999999999486395175, 0.3999999999315194676, 0.5999999999315199783, 1.000000000000000000),
 ( 0.2500000000000000000, 0.2499999999657600003, 0.2999999999486395175, 0.3999999999315194676, 0.5999999999315199783, 1.000000000000000000) ) ) 
 REPRESENTATION_ITEM ( '' )  SURFACE ( )  );
#12964 = CARTESIAN_POINT ( 'NONE',  ( -27.13030197561320733, 35.14114750801761033, -148.0149677930219525 ) ) ;
#12965 = CARTESIAN_POINT ( 'NONE',  ( 16.29836742280000195, -22.74229684829999698, -143.5552959529999839 ) ) ;
#12966 = CARTESIAN_POINT ( 'NONE',  ( -12.28014746100000032, 36.97113097969999984, -148.4919582129999753 ) ) ;
#12967 = DIRECTION ( 'NONE',  ( -2.257144641399999941E-12, 0.000000000000000000, -1.000000000000000000 ) ) ;
#12968 = VECTOR ( 'NONE', #6901, 1000.000000000000000 ) ;
#12969 = CARTESIAN_POINT ( 'NONE',  ( -11.38486064709999823, 36.95668670079999885, -140.3965526140000009 ) ) ;
#12970 = VECTOR ( 'NONE', #14585, 1000.000000000000000 ) ;
#12971 = AXIS2_PLACEMENT_3D ( 'NONE', #16455, #11429, #20721 ) ;
#12972 = ORIENTED_EDGE ( 'NONE', *, *, #9437, .T. ) ;
#12973 = EDGE_CURVE ( 'NONE', #10427, #1513, #14756, .T. ) ;
#12974 = CARTESIAN_POINT ( 'NONE',  ( 9.882881882281347785, -21.11395234859968184, -148.5552959529999839 ) ) ;
#12975 = CARTESIAN_POINT ( 'NONE',  ( -31.00000000000000000, 26.50000000000000000, -149.0552959529999839 ) ) ;
#12976 = ORIENTED_EDGE ( 'NONE', *, *, #605, .F. ) ;
#12977 = EDGE_CURVE ( 'NONE', #2789, #18478, #22253, .T. ) ;
#12978 = VERTEX_POINT ( 'NONE', #13318 ) ;
#12979 = DIRECTION ( 'NONE',  ( -1.000000000000000000, 0.000000000000000000, 2.257144641399999941E-12 ) ) ;
#12980 = DIRECTION ( 'NONE',  ( 0.000000000000000000, -1.000000000000000000, 0.000000000000000000 ) ) ;
#12981 = DIRECTION ( 'NONE',  ( 0.000000000000000000, 1.000000000000000000, 0.000000000000000000 ) ) ;
#12982 = CARTESIAN_POINT ( 'NONE',  ( 32.50000000000000000, 32.96379895120000469, -136.5552959530000123 ) ) ;
#12983 = ORIENTED_EDGE ( 'NONE', *, *, #1401, .F. ) ;
#12984 = DIRECTION ( 'NONE',  ( -2.252420472359999842E-12, 0.000000000000000000, 1.000000000000000000 ) ) ;
#12985 = AXIS2_PLACEMENT_3D ( 'NONE', #3606, #7401, #8937 ) ;
#12986 = VECTOR ( 'NONE', #11434, 1000.000000000000000 ) ;
#12987 = CARTESIAN_POINT ( 'NONE',  ( -18.01531055826208672, 36.06437412970446132, -148.3642685968914634 ) ) ;
#12988 = VECTOR ( 'NONE', #10352, 1000.000000000000000 ) ;
#12989 = FACE_OUTER_BOUND ( 'NONE', #16375, .T. ) ;
#12990 = FACE_OUTER_BOUND ( 'NONE', #6165, .T. ) ;
#12991 = CARTESIAN_POINT ( 'NONE',  ( -24.91068290195174129, 38.76331891718528766, -147.9212516401705386 ) ) ;
#12992 = EDGE_CURVE ( 'NONE', #3932, #10783, #2507, .T. ) ;
#12993 = CARTESIAN_POINT ( 'NONE',  ( -15.56194485763432134, 32.85813890014918570, -144.2218690930858145 ) ) ;
#12994 = DIRECTION ( 'NONE',  ( -2.507771768019999718E-12, -1.592654864069999939E-17, 1.000000000000000000 ) ) ;
#12995 = DIRECTION ( 'NONE',  ( 0.000000000000000000, 0.000000000000000000, -1.000000000000000000 ) ) ;
#12996 = LINE ( 'NONE', #15372, #22584 ) ;
#12997 = EDGE_CURVE ( 'NONE', #15090, #10047, #6925, .T. ) ;
#12998 = VERTEX_POINT ( 'NONE', #20699 ) ;
#12999 = CARTESIAN_POINT ( 'NONE',  ( -5.345822467930000599, 40.94956462150000220, -144.4907973060000188 ) ) ;
#13000 = VECTOR ( 'NONE', #15442, 1000.000000000000114 ) ;
#13001 = AXIS2_PLACEMENT_3D ( 'NONE', #15482, #20844, #2648 ) ;
#13002 = ORIENTED_EDGE ( 'NONE', *, *, #13104, .F. ) ;
#13003 = AXIS2_PLACEMENT_3D ( 'NONE', #6758, #2621, #953 ) ;
#13004 = DIRECTION ( 'NONE',  ( 0.000000000000000000, -1.000000000000000000, 0.000000000000000000 ) ) ;
#13005 = ADVANCED_FACE ( 'NONE', ( #2281 ), #9270, .T. ) ;
#13006 = DIRECTION ( 'NONE',  ( 2.839308199620000013E-14, 3.568879590630000244E-13, 1.000000000000000000 ) ) ;
#13007 = FACE_OUTER_BOUND ( 'NONE', #16276, .T. ) ;
#13008 = ORIENTED_EDGE ( 'NONE', *, *, #21868, .T. ) ;
#13009 = CARTESIAN_POINT ( 'NONE',  ( -13.15660544825068712, 35.28848928018297926, -140.1477172601388190 ) ) ;
#13010 = LINE ( 'NONE', #11096, #12763 ) ;
#13011 = CARTESIAN_POINT ( 'NONE',  ( 13.09818317338255156, 38.33939095839281208, -150.0552959529999839 ) ) ;
#13012 = CARTESIAN_POINT ( 'NONE',  ( -30.49999999990000177, 47.50000000000000000, -147.5552959529999839 ) ) ;
#13013 = CARTESIAN_POINT ( 'NONE',  ( -18.07392865170000107, -34.50000000000000000, -147.3157682190000060 ) ) ;
#13014 = CARTESIAN_POINT ( 'NONE',  ( 3.579871919197813224, -4.701030550647564255, -136.0552959530081125 ) ) ;
#13015 = EDGE_CURVE ( 'NONE', #16420, #21462, #367, .T. ) ;
#13016 = EDGE_LOOP ( 'NONE', ( #21397, #19986, #11314, #8143 ) ) ;
#13017 = STYLED_ITEM ( 'NONE', ( #16831 ), #8081 ) ;
#13018 = EDGE_CURVE ( 'NONE', #9539, #11240, #4288, .T. ) ;
#13019 = CIRCLE ( 'NONE', #9590, 1.000000000000000888 ) ;
#13020 = CARTESIAN_POINT ( 'NONE',  ( -27.81458217780672726, 35.04316096251904611, -148.4325824290839364 ) ) ;
#13021 = EDGE_LOOP ( 'NONE', ( #12003, #9898, #1082, #7426, #15093 ) ) ;
#13022 = ORIENTED_EDGE ( 'NONE', *, *, #1412, .F. ) ;
#13023 = CARTESIAN_POINT ( 'NONE',  ( -12.47706116150000000, 35.17890886639999337, -148.2557368829999973 ) ) ;
#13024 = PLANE ( 'NONE',  #9560 ) ;
#13025 = CARTESIAN_POINT ( 'NONE',  ( 17.33131581010000133, -22.98361965280000163, -147.0552959529999839 ) ) ;
#13026 = EDGE_CURVE ( 'NONE', #11018, #16936, #18445, .T. ) ;
#13027 = ORIENTED_EDGE ( 'NONE', *, *, #3588, .T. ) ;
#13028 = CARTESIAN_POINT ( 'NONE',  ( -33.50000000000000000, 26.00000000000000000, -150.5552959529999839 ) ) ;
#13029 = DIRECTION ( 'NONE',  ( 2.258193632089999862E-12, 0.000000000000000000, 1.000000000000000000 ) ) ;
#13030 = EDGE_CURVE ( 'NONE', #3680, #3138, #5712, .T. ) ;
#13031 = CYLINDRICAL_SURFACE ( 'NONE', #5641, 6.000000000000003553 ) ;
#13032 = VERTEX_POINT ( 'NONE', #20245 ) ;
#13033 = CARTESIAN_POINT ( 'NONE',  ( -21.31444489898548866, 40.98951650670894509, -143.6265206826709004 ) ) ;
#13034 = EDGE_CURVE ( 'NONE', #19256, #2929, #2398, .T. ) ;
#13035 = ADVANCED_FACE ( 'NONE', ( #15105 ), #5825, .F. ) ;
#13036 = CARTESIAN_POINT ( 'NONE',  ( -16.81794493320086303, 37.02435727938927812, -140.5111119822732064 ) ) ;
#13037 = STYLED_ITEM ( 'NONE', ( #485 ), #5808 ) ;
#13038 = CARTESIAN_POINT ( 'NONE',  ( -32.50000000000000000, -50.00000000000000000, -143.3052959529999839 ) ) ;
#13039 = DIRECTION ( 'NONE',  ( 0.000000000000000000, -1.000000000000000000, 0.000000000000000000 ) ) ;
#13040 = ORIENTED_EDGE ( 'NONE', *, *, #8353, .T. ) ;
#13041 = CARTESIAN_POINT ( 'NONE',  ( 10.93320006080000084, 3.500000000000000000, -150.0552959529999839 ) ) ;
#13042 = ORIENTED_EDGE ( 'NONE', *, *, #21584, .F. ) ;
#13043 = CARTESIAN_POINT ( 'NONE',  ( 8.351115582531676296, -48.22632467507040133, -150.0552959529999839 ) ) ;
#13044 = ORIENTED_EDGE ( 'NONE', *, *, #7784, .F. ) ;
#13045 = CARTESIAN_POINT ( 'NONE',  ( -26.65693523154040534, 40.12876521656455964, -145.8849180162604000 ) ) ;
#13046 = ORIENTED_EDGE ( 'NONE', *, *, #3709, .T. ) ;
#13047 = CARTESIAN_POINT ( 'NONE',  ( -21.48110840330020466, 32.98389871696830511, -146.2328788545872271 ) ) ;
#13048 = ORIENTED_EDGE ( 'NONE', *, *, #13677, .F. ) ;
#13049 = CARTESIAN_POINT ( 'NONE',  ( -8.650148125288117384, -11.23751091877166886, -145.5552959530002965 ) ) ;
#13050 = EDGE_LOOP ( 'NONE', ( #19222, #7315, #20732, #20309 ) ) ;
#13051 = APPLICATION_PROTOCOL_DEFINITION ( 'draft international standard', 'automotive_design', 1998, #7803 ) ;
#13052 = ORIENTED_EDGE ( 'NONE', *, *, #10074, .F. ) ;
#13053 = B_SPLINE_CURVE_WITH_KNOTS ( 'NONE', 3,
 ( #3939, #17005, #2399, #4290 ),
 .UNSPECIFIED., .F., .F.,
 ( 4, 4 ),
 ( 0.000000000000000000, 0.8059436278830001132 ),
 .UNSPECIFIED. ) ;
#13054 = CARTESIAN_POINT ( 'NONE',  ( -28.06178240320601347, 37.06443177825870094, -147.7991814975441685 ) ) ;
#13055 = CARTESIAN_POINT ( 'NONE',  ( -14.58162373620000096, 40.18882273020000184, -142.1871799649999843 ) ) ;
#13056 = ADVANCED_FACE ( 'NONE', ( #9851 ), #15579, .T. ) ;
#13057 = LINE ( 'NONE', #4021, #19089 ) ;
#13058 = CARTESIAN_POINT ( 'NONE',  ( -19.86630785130000021, -51.50000000000000000, -137.0552959530000123 ) ) ;
#13059 = DIRECTION ( 'NONE',  ( 1.000000000000000000, 0.000000000000000000, 0.000000000000000000 ) ) ;
#13060 = DIRECTION ( 'NONE',  ( 0.000000000000000000, -1.000000000000000000, 0.000000000000000000 ) ) ;
#13061 = ORIENTED_EDGE ( 'NONE', *, *, #7468, .F. ) ;
#13062 = CARTESIAN_POINT ( 'NONE',  ( -21.35824191589999899, -32.00000000000000000, -141.0657682190000060 ) ) ;
#13063 = CARTESIAN_POINT ( 'NONE',  ( -7.041959465309999722, -26.08051538799999847, -142.5552959529999839 ) ) ;
#13064 = ORIENTED_EDGE ( 'NONE', *, *, #6985, .T. ) ;
#13065 = LINE ( 'NONE', #233, #9736 ) ;
#13066 = CARTESIAN_POINT ( 'NONE',  ( -12.91895806490169996, 38.59375950464521310, -147.5965526133004460 ) ) ;
#13067 = VECTOR ( 'NONE', #873, 1000.000000000000000 ) ;
#13068 = DIRECTION ( 'NONE',  ( -1.211690350419999855E-27, -2.765629237170000203E-27, 1.000000000000000000 ) ) ;
#13069 = CARTESIAN_POINT ( 'NONE',  ( -29.88845675159999971, 40.47687533140000227, -144.8298193859999969 ) ) ;
#13070 = ORIENTED_EDGE ( 'NONE', *, *, #8103, .F. ) ;
#13071 = CARTESIAN_POINT ( 'NONE',  ( -7.220568065030000149, 34.52259161599999970, -140.6708207100000152 ) ) ;
#13072 = CARTESIAN_POINT ( 'NONE',  ( 2.499999999879999990, -3.000000000000000000, -135.0552959530000123 ) ) ;
#13073 = ORIENTED_EDGE ( 'NONE', *, *, #279, .F. ) ;
#13074 = CARTESIAN_POINT ( 'NONE',  ( 16.25412235410000150, -22.59491385829999999, -145.5552959529999839 ) ) ;
#13075 = CARTESIAN_POINT ( 'NONE',  ( -0.6781431574009999519, -62.17334590100000469, -147.5552959529999839 ) ) ;
#13076 = DIRECTION ( 'NONE',  ( -2.507771768019999718E-12, -1.592654864069999939E-17, 1.000000000000000000 ) ) ;
#13077 = CARTESIAN_POINT ( 'NONE',  ( -20.13480534186356508, 38.99445981612083045, -139.6568722183936018 ) ) ;
#13078 = ORIENTED_EDGE ( 'NONE', *, *, #15724, .F. ) ;
#13079 = CARTESIAN_POINT ( 'NONE',  ( 25.15155135439999867, -26.08415009650000016, -147.5552959529999839 ) ) ;
#13080 = ADVANCED_FACE ( 'NONE', ( #17480 ), #8428, .T. ) ;
#13081 = EDGE_LOOP ( 'NONE', ( #22121, #15912, #22669, #5233 ) ) ;
#13082 = FACE_OUTER_BOUND ( 'NONE', #6344, .T. ) ;
#13083 = CARTESIAN_POINT ( 'NONE',  ( -21.35824191589999899, -4.000000000000000000, -144.8157682190000060 ) ) ;
#13084 = ADVANCED_FACE ( 'NONE', ( #19391 ), #4747, .F. ) ;
#13085 = CARTESIAN_POINT ( 'NONE',  ( -10.66194399679999982, 33.15920395730000081, -144.2988335299999960 ) ) ;
#13086 = EDGE_LOOP ( 'NONE', ( #3256, #205, #16731, #2357, #2965, #16369 ) ) ;
#13087 = VECTOR ( 'NONE', #14538, 1000.000000000000000 ) ;
#13088 = CARTESIAN_POINT ( 'NONE',  ( -20.21101409811914706, 36.97743810397754771, -140.7155889590011952 ) ) ;
#13089 = DIRECTION ( 'NONE',  ( 2.257171095940000041E-12, 1.003664318210000046E-28, 1.000000000000000000 ) ) ;
#13090 = EDGE_LOOP ( 'NONE', ( #18693, #21581, #21319, #2542, #12072 ) ) ;
#13091 = VERTEX_POINT ( 'NONE', #8302 ) ;
#13092 = CARTESIAN_POINT ( 'NONE',  ( -23.41786221899999987, 36.12684018730000446, -140.1150171360000058 ) ) ;
#13093 = LINE ( 'NONE', #20364, #21907 ) ;
#13094 = CARTESIAN_POINT ( 'NONE',  ( -22.42941481619999777, 36.22509709909999742, -139.9955747719999692 ) ) ;
#13095 = CARTESIAN_POINT ( 'NONE',  ( 7.817303505803055330, 35.66414413158247498, -141.9420359948146881 ) ) ;
#13096 = ORIENTED_EDGE ( 'NONE', *, *, #5592, .F. ) ;
#13097 = DIRECTION ( 'NONE',  ( 1.267807176944654053E-15, 0.000000000000000000, 1.000000000000000000 ) ) ;
#13098 = CARTESIAN_POINT ( 'NONE',  ( 20.35976161480000002, -31.74228192520000391, -145.5552959529999839 ) ) ;
#13099 = CARTESIAN_POINT ( 'NONE',  ( -32.50000000000000000, -36.00000000000000000, -149.5552959529999839 ) ) ;
#13100 = FACE_OUTER_BOUND ( 'NONE', #14992, .T. ) ;
#13101 = CARTESIAN_POINT ( 'NONE',  ( -24.97797643630000053, 37.05442817780000553, -147.8575004449999994 ) ) ;
#13102 = VECTOR ( 'NONE', #9013, 1000.000000000000000 ) ;
#13103 = CARTESIAN_POINT ( 'NONE',  ( -16.17059658477510808, 32.32997518586915220, -143.3112915338346909 ) ) ;
#13104 = EDGE_CURVE ( 'NONE', #3115, #20005, #1203, .T. ) ;
#13105 = CARTESIAN_POINT ( 'NONE',  ( 19.13369214859999801, 50.50000000000000000, -136.0552959530000123 ) ) ;
#13106 = DIRECTION ( 'NONE',  ( 0.09606172499277226828, 0.9953753789357124848, -8.277822871607614780E-13 ) ) ;
#13107 = ADVANCED_FACE ( 'NONE', ( #4866 ), #22712, .F. ) ;
#13108 = CARTESIAN_POINT ( 'NONE',  ( 24.36715301250000110, -30.57462384669999977, -147.5552959529999839 ) ) ;
#13109 = ORIENTED_EDGE ( 'NONE', *, *, #11557, .F. ) ;
#13110 = CARTESIAN_POINT ( 'NONE',  ( -5.777804233054069094, 40.42495531994817526, -144.3912056291562180 ) ) ;
#13111 = CARTESIAN_POINT ( 'NONE',  ( 7.200097415480000151, -13.39991276200000136, -144.5552959529999839 ) ) ;
#13112 = ORIENTED_EDGE ( 'NONE', *, *, #8152, .F. ) ;
#13113 = PRESENTATION_STYLE_ASSIGNMENT (( #5627 ) ) ;
#13114 = ORIENTED_CLOSED_SHELL ( 'NONE', *, #6122, .F. );
#13116 = CIRCLE ( 'NONE', #16176, 3.000000000000000888 ) ;
#13115 = CARTESIAN_POINT ( 'NONE',  ( -22.18638062229441132, 34.91229655975453028, -146.9294338459641551 ) ) ;
#13117 = AXIS2_PLACEMENT_3D ( 'NONE', #12796, #16267, #7554 ) ;
#13118 = CARTESIAN_POINT ( 'NONE',  ( 8.100000000049998761, 39.46779253580000102, -149.5552959529999839 ) ) ;
#13119 = ORIENTED_EDGE ( 'NONE', *, *, #12946, .F. ) ;
#13120 = CARTESIAN_POINT ( 'NONE',  ( -13.43635516220704318, 34.87491094518600931, -141.2152170337695622 ) ) ;
#13121 = LINE ( 'NONE', #11322, #11232 ) ;
#13122 = PLANE ( 'NONE',  #19649 ) ;
#13123 = DIRECTION ( 'NONE',  ( 2.257144641399999941E-12, 0.000000000000000000, -1.000000000000000000 ) ) ;
#13124 = CARTESIAN_POINT ( 'NONE',  ( -32.50000000000000000, -64.50000000000000000, -144.0552959529999839 ) ) ;
#13125 = EDGE_CURVE ( 'NONE', #8795, #12291, #19029, .T. ) ;
#13126 = CARTESIAN_POINT ( 'NONE',  ( 4.020454867573966418, -37.28105831637246581, -150.0552959530000123 ) ) ;
#13127 = APPLICATION_CONTEXT ( 'automotive_design' ) ;
#13128 = EDGE_LOOP ( 'NONE', ( #18917, #2608, #4696, #19829 ) ) ;
#13129 = CARTESIAN_POINT ( 'NONE',  ( -27.58110728279703849, 34.24318910290035944, -147.7245096245254103 ) ) ;
#13130 = EDGE_LOOP ( 'NONE', ( #14979, #7573, #19557, #17532, #17754, #3763, #22896, #21004 ) ) ;
#13131 = ORIENTED_EDGE ( 'NONE', *, *, #20741, .F. ) ;
#13132 = AXIS2_PLACEMENT_3D ( 'NONE', #17112, #832, #6278 ) ;
#13133 = CARTESIAN_POINT ( 'NONE',  ( -13.92432874550000044, 37.01165864720000087, -139.5650670249999905 ) ) ;
#13134 = CARTESIAN_POINT ( 'NONE',  ( -4.499999999969999109, 37.00000000000000000, -137.0552959530000123 ) ) ;
#13135 = EDGE_CURVE ( 'NONE', #6792, #2284, #10714, .T. ) ;
#13136 = AXIS2_PLACEMENT_3D ( 'NONE', #6952, #7071, #3382 ) ;
#13137 = CARTESIAN_POINT ( 'NONE',  ( 5.631397321050000571, -17.85059010000000157, -146.5552959529999839 ) ) ;
#13138 = ORIENTED_EDGE ( 'NONE', *, *, #11833, .T. ) ;
#13139 = LINE ( 'NONE', #11464, #15180 ) ;
#13140 = CARTESIAN_POINT ( 'NONE',  ( 12.77456842470000176, -18.14116071520000162, -142.5552959529999839 ) ) ;
#13141 = VERTEX_POINT ( 'NONE', #22841 ) ;
#13142 = CARTESIAN_POINT ( 'NONE',  ( 1.591914056710000080, -18.48847405160000079, -144.5552959529999839 ) ) ;
#13143 = EDGE_CURVE ( 'NONE', #5200, #19847, #4987, .T. ) ;
#13144 = CARTESIAN_POINT ( 'NONE',  ( 9.447876141023428431, 38.16353938488455810, -141.8420144859424568 ) ) ;
#13145 = AXIS2_PLACEMENT_3D ( 'NONE', #13809, #15707, #4759 ) ;
#13146 = CARTESIAN_POINT ( 'NONE',  ( -2.500000000000000000, 34.00000000000000000, -150.0552959529999839 ) ) ;
#13147 = AXIS2_PLACEMENT_3D ( 'NONE', #3018, #21102, #12158 ) ;
#13148 = EDGE_LOOP ( 'NONE', ( #19959, #5275, #21354, #16886, #7665, #2400, #14917, #8389, #13922, #4879, #12962, #20798 ) ) ;
#13149 = ADVANCED_FACE ( 'NONE', ( #6645 ), #20625, .F. ) ;
#13150 = ADVANCED_FACE ( 'NONE', ( #21061 ), #4636, .F. ) ;
#13151 = PLANE ( 'NONE',  #19036 ) ;
#13152 = ORIENTED_EDGE ( 'NONE', *, *, #11564, .F. ) ;
#13153 = EDGE_CURVE ( 'NONE', #15515, #1286, #10343, .T. ) ;
#13154 = VERTEX_POINT ( 'NONE', #843 ) ;
#13155 = CARTESIAN_POINT ( 'NONE',  ( -27.48801997220000004, 39.21796412529999998, -147.0196846460000017 ) ) ;
#13156 = ORIENTED_EDGE ( 'NONE', *, *, #10533, .T. ) ;
#13157 = CARTESIAN_POINT ( 'NONE',  ( -31.50000000000000000, 10.25000000000000000, -149.5552959529999839 ) ) ;
#13158 = EDGE_CURVE ( 'NONE', #19654, #23517, #8537, .T. ) ;
#13159 = ORIENTED_EDGE ( 'NONE', *, *, #5754, .T. ) ;
#13160 = FACE_OUTER_BOUND ( 'NONE', #19473, .T. ) ;
#13161 = ORIENTED_EDGE ( 'NONE', *, *, #5935, .F. ) ;
#13162 = APPLICATION_PROTOCOL_DEFINITION ( 'draft international standard', 'automotive_design', 1998, #22107 ) ;
#13163 = VERTEX_POINT ( 'NONE', #1071 ) ;
#13164 = DIRECTION ( 'NONE',  ( 0.000000000000000000, 0.000000000000000000, -1.000000000000000000 ) ) ;
#13165 = DIRECTION ( 'NONE',  ( -0.7633862853691523176, 0.6459422414661291079, 0.000000000000000000 ) ) ;
#13166 = VECTOR ( 'NONE', #17612, 1000.000000000000000 ) ;
#13167 = CARTESIAN_POINT ( 'NONE',  ( -30.49999999990000177, 45.00000000000000000, -144.0552959529999839 ) ) ;
#13168 = CARTESIAN_POINT ( 'NONE',  ( 12.50000000010000001, 16.89444872450000190, -143.5552959529999839 ) ) ;
#13169 = CARTESIAN_POINT ( 'NONE',  ( -7.206173031983939659, 35.38491483748016009, -147.9515367334090001 ) ) ;
#13170 = CARTESIAN_POINT ( 'NONE',  ( -32.50000000000000000, 50.00000000000000000, -150.5552959529999839 ) ) ;
#13171 = EDGE_LOOP ( 'NONE', ( #1167, #23393, #12839, #1457 ) ) ;
#13172 = CARTESIAN_POINT ( 'NONE',  ( -18.35824191589999899, -18.00000000000000000, -150.0657682190000060 ) ) ;
#13173 = LINE ( 'NONE', #20446, #22777 ) ;
#13174 = CARTESIAN_POINT ( 'NONE',  ( 31.50000000000000000, -40.03620104880000241, -149.5552959529999839 ) ) ;
#13175 = VERTEX_POINT ( 'NONE', #21296 ) ;
#13176 = EDGE_CURVE ( 'NONE', #7834, #10448, #17603, .T. ) ;
#13177 = CARTESIAN_POINT ( 'NONE',  ( -12.57385931471914198, 38.47543513197548037, -147.4253642441603915 ) ) ;
#13178 = ADVANCED_FACE ( 'NONE', ( #17126 ), #10080, .F. ) ;
#13179 = CARTESIAN_POINT ( 'NONE',  ( -18.75277607359999976, 37.97046254950000588, -148.4181951110000171 ) ) ;
#13180 = CARTESIAN_POINT ( 'NONE',  ( -29.55751743908506413, 40.46053532644847195, -144.8661948876702752 ) ) ;
#13181 = VECTOR ( 'NONE', #11185, 1000.000000000000227 ) ;
#13182 = ORIENTED_EDGE ( 'NONE', *, *, #13727, .F. ) ;
#13183 = CARTESIAN_POINT ( 'NONE',  ( -6.033650297970000409, 36.94170754819999303, -147.9652040070000112 ) ) ;
#13184 = FACE_OUTER_BOUND ( 'NONE', #3886, .T. ) ;
#13185 = ORIENTED_EDGE ( 'NONE', *, *, #20450, .T. ) ;
#13186 = DIRECTION ( 'NONE',  ( 1.527666881879999979E-13, 8.153477892850000134E-13, 1.000000000000000000 ) ) ;
#13187 = CARTESIAN_POINT ( 'NONE',  ( -8.770737564319999180, -11.35481373070000011, -143.5552959529999839 ) ) ;
#13188 = ORIENTED_EDGE ( 'NONE', *, *, #14649, .T. ) ;
#13189 = CARTESIAN_POINT ( 'NONE',  ( -8.916553640509999212, -11.88594259849999979, -142.5552959529999839 ) ) ;
#13190 = CARTESIAN_POINT ( 'NONE',  ( -20.90770409063893354, 39.73774297846755843, -147.9490349955885620 ) ) ;
#13191 = ORIENTED_EDGE ( 'NONE', *, *, #20608, .T. ) ;
#13192 = CARTESIAN_POINT ( 'NONE',  ( -27.07034204102121322, 35.31393907231532125, -147.6133383737439431 ) ) ;
#13193 = CYLINDRICAL_SURFACE ( 'NONE', #11027, 2.999999999999999112 ) ;
#13194 = ORIENTED_EDGE ( 'NONE', *, *, #20324, .T. ) ;
#13195 = CARTESIAN_POINT ( 'NONE',  ( 0.5000000001590285681, 16.89444872450000190, -139.5552959529864268 ) ) ;
#13196 = LINE ( 'NONE', #3937, #11076 ) ;
#13197 = DIRECTION ( 'NONE',  ( 2.507771768019999718E-12, 1.592654864209999947E-17, -1.000000000000000000 ) ) ;
#13198 = AXIS2_PLACEMENT_3D ( 'NONE', #22234, #11499, #18778 ) ;
#13199 = VERTEX_POINT ( 'NONE', #15453 ) ;
#13200 = CARTESIAN_POINT ( 'NONE',  ( 0.5000000001659999915, 20.50000000000000000, -136.5552959530000123 ) ) ;
#13201 = VECTOR ( 'NONE', #12097, 1000.000000000000000 ) ;
#13202 = CARTESIAN_POINT ( 'NONE',  ( -3.234790887152434458, 46.50000000000001421, -136.0552959529926795 ) ) ;
#13203 = ORIENTED_EDGE ( 'NONE', *, *, #10649, .T. ) ;
#13204 = ORIENTED_EDGE ( 'NONE', *, *, #11688, .F. ) ;
#13205 = CARTESIAN_POINT ( 'NONE',  ( -21.35824191589999899, -4.000000000000000000, -146.2257682199999920 ) ) ;
#13206 = EDGE_CURVE ( 'NONE', #18341, #3836, #17356, .T. ) ;
#13207 = CARTESIAN_POINT ( 'NONE',  ( -21.35824191589999899, -31.25000000000000000, -144.8157682190000060 ) ) ;
#13208 = FACE_OUTER_BOUND ( 'NONE', #9159, .T. ) ;
#13209 = CARTESIAN_POINT ( 'NONE',  ( 8.085152496479286910, 35.55829573485724637, -142.0128484172198853 ) ) ;
#13210 = EDGE_LOOP ( 'NONE', ( #5325, #20381, #5262, #1768 ) ) ;
#13211 = PLANE ( 'NONE',  #14715 ) ;
#13212 = CARTESIAN_POINT ( 'NONE',  ( -7.529689113779999943, 37.05876528330000497, -139.9906690790000141 ) ) ;
#13213 = AXIS2_PLACEMENT_3D ( 'NONE', #2066, #2301, #9174 ) ;
#13214 = DIRECTION ( 'NONE',  ( 9.185449151653098762E-12, 0.000000000000000000, 1.000000000000000000 ) ) ;
#13215 = CARTESIAN_POINT ( 'NONE',  ( 12.49993271309136311, 36.89748944249159024, -136.0552959530282635 ) ) ;
#13216 = CARTESIAN_POINT ( 'NONE',  ( -23.76507348473139913, 39.47303768189023998, -147.6024660349875717 ) ) ;
#13217 = AXIS2_PLACEMENT_3D ( 'NONE', #2466, #10037, #6135 ) ;
#13218 = CARTESIAN_POINT ( 'NONE',  ( -15.14562011634022731, 35.04295422807219040, -148.0905764885102371 ) ) ;
#13219 = CARTESIAN_POINT ( 'NONE',  ( -16.92867099909999595, 34.38083942290000294, -140.2753207150000208 ) ) ;
#13220 = LINE ( 'NONE', #17028, #22117 ) ;
#13221 = DIRECTION ( 'NONE',  ( 0.000000000000000000, -1.000000000000000000, 0.000000000000000000 ) ) ;
#13222 = CARTESIAN_POINT ( 'NONE',  ( -18.07392865170000107, -18.00000000000000000, -144.8157682190000060 ) ) ;
#13223 = EDGE_LOOP ( 'NONE', ( #14938, #10374, #12782, #1654, #4511 ) ) ;
#13224 = CARTESIAN_POINT ( 'NONE',  ( -6.787442408928496818, 39.33311790174365541, -147.1061528123235860 ) ) ;
#13225 = FACE_BOUND ( 'NONE', #14080, .T. ) ;
#13226 = EDGE_LOOP ( 'NONE', ( #4220, #15333 ) ) ;
#13227 = DIRECTION ( 'NONE',  ( -0.07970438983373198671, -0.9968185442904001770, 8.248698894599408818E-13 ) ) ;
#13228 = AXIS2_PLACEMENT_3D ( 'NONE', #3233, #10467, #3008 ) ;
#13229 = VECTOR ( 'NONE', #8094, 1000.000000000000000 ) ;
#13230 = CARTESIAN_POINT ( 'NONE',  ( -21.12162747660223872, 36.95220905035969139, -147.5578847871684900 ) ) ;
#13231 = CARTESIAN_POINT ( 'NONE',  ( 4.750000000030000002, -44.75000000000000000, -136.5552959530000123 ) ) ;
#13232 = ORIENTED_EDGE ( 'NONE', *, *, #9437, .F. ) ;
#13233 = DIRECTION ( 'NONE',  ( 0.000000000000000000, 0.000000000000000000, 1.000000000000000000 ) ) ;
#13234 = EDGE_CURVE ( 'NONE', #15683, #22142, #7001, .T. ) ;
#13235 = ADVANCED_FACE ( 'NONE', ( #19859 ), #5457, .T. ) ;
#13236 = CARTESIAN_POINT ( 'NONE',  ( -16.92431971702843541, 37.01165972487795131, -139.4624774945204422 ) ) ;
#13237 = AXIS2_PLACEMENT_3D ( 'NONE', #2052, #7387, #14293 ) ;
#13238 = CARTESIAN_POINT ( 'NONE',  ( -37.07045745269999770, 26.50000000000000000, -139.0687076600000012 ) ) ;
#13239 = PLANE ( 'NONE',  #8619 ) ;
#13240 = EDGE_CURVE ( 'NONE', #16530, #2118, #19365, .T. ) ;
#13241 = CARTESIAN_POINT ( 'NONE',  ( 29.68320006080000084, 0.9999999999989999111, -150.0552959529999839 ) ) ;
#13242 = CARTESIAN_POINT ( 'NONE',  ( 3.742569615074119671, -4.809943152218662199, -136.0552959530084536 ) ) ;
#13243 = ORIENTED_EDGE ( 'NONE', *, *, #8513, .F. ) ;
#13244 = CARTESIAN_POINT ( 'NONE',  ( -28.77360867277181811, 32.46091987502819620, -144.5371065550806975 ) ) ;
#13245 = AXIS2_PLACEMENT_3D ( 'NONE', #22943, #19363, #817 ) ;
#13246 = CIRCLE ( 'NONE', #2269, 2.500000000000000444 ) ;
#13247 = VERTEX_POINT ( 'NONE', #15331 ) ;
#13248 = CARTESIAN_POINT ( 'NONE',  ( -14.21072043115257699, 34.69090590940501784, -141.1210154221530786 ) ) ;
#13249 = FACE_OUTER_BOUND ( 'NONE', #12470, .T. ) ;
#13250 = LINE ( 'NONE', #13373, #18393 ) ;
#13251 = CIRCLE ( 'NONE', #1509, 0.7500000000000006661 ) ;
#13252 = ORIENTED_EDGE ( 'NONE', *, *, #5754, .F. ) ;
#13253 = VECTOR ( 'NONE', #21803, 1000.000000000000000 ) ;
#13254 = CARTESIAN_POINT ( 'NONE',  ( 22.40528270640000130, -21.39206583629999869, -146.5552959529999839 ) ) ;
#13255 = CYLINDRICAL_SURFACE ( 'NONE', #3049, 2.000000000000003553 ) ;
#13256 = VERTEX_POINT ( 'NONE', #10671 ) ;
#13257 = LINE ( 'NONE', #13142, #20536 ) ;
#13258 = CARTESIAN_POINT ( 'NONE',  ( 9.339387736956417996, 38.24315306418434091, -141.8862908787521633 ) ) ;
#13259 = VECTOR ( 'NONE', #4208, 1000.000000000000114 ) ;
#13260 = FACE_OUTER_BOUND ( 'NONE', #12210, .T. ) ;
#13261 = CARTESIAN_POINT ( 'NONE',  ( 22.00000000000000000, -20.50000000000000000, -136.0552959530000123 ) ) ;
#13262 = EDGE_CURVE ( 'NONE', #21613, #16855, #16405, .T. ) ;
#13263 = VERTEX_POINT ( 'NONE', #21771 ) ;
#13264 = AXIS2_PLACEMENT_3D ( 'NONE', #21413, #15699, #8300 ) ;
#13265 = CIRCLE ( 'NONE', #6433, 9.999999999999998224 ) ;
#13266 = PLANE ( 'NONE',  #22851 ) ;
#13267 = VERTEX_POINT ( 'NONE', #3672 ) ;
#13268 = LINE ( 'NONE', #4007, #4103 ) ;
#13269 = ORIENTED_EDGE ( 'NONE', *, *, #5315, .T. ) ;
#13270 = LINE ( 'NONE', #1031, #14151 ) ;
#13271 = ORIENTED_EDGE ( 'NONE', *, *, #8938, .T. ) ;
#13272 = CARTESIAN_POINT ( 'NONE',  ( -9.395847196590883854, -17.80940328571869102, -146.5552959529997565 ) ) ;
#13273 = EDGE_CURVE ( 'NONE', #21143, #16352, #10785, .T. ) ;
#13274 = VERTEX_POINT ( 'NONE', #3437 ) ;
#13275 = DIRECTION ( 'NONE',  ( 0.000000000000000000, -1.000000000000000000, 0.000000000000000000 ) ) ;
#13276 = ORIENTED_EDGE ( 'NONE', *, *, #19570, .F. ) ;
#13277 = CIRCLE ( 'NONE', #3045, 1.499999999999999556 ) ;
#13278 = ORIENTED_EDGE ( 'NONE', *, *, #19647, .T. ) ;
#13279 = CARTESIAN_POINT ( 'NONE',  ( -28.08093528158016383, 37.94476457440455164, -148.1477062081667668 ) ) ;
#13280 = DIRECTION ( 'NONE',  ( 1.000000000000000000, 0.000000000000000000, 0.000000000000000000 ) ) ;
#13281 = CARTESIAN_POINT ( 'NONE',  ( 1.357896944619999990, -19.89221232270000073, -148.0552959529999839 ) ) ;
#13282 = CARTESIAN_POINT ( 'NONE',  ( -0.6781431574009999519, -62.17334590100000469, -147.5552959529999839 ) ) ;
#13283 = AXIS2_PLACEMENT_3D ( 'NONE', #6852, #21149, #13635 ) ;
#13284 = AXIS2_PLACEMENT_3D ( 'NONE', #9128, #5215, #18072 ) ;
#13285 = DIRECTION ( 'NONE',  ( -0.7633862853691524286, -0.6459422414661292189, 5.745404152441153618E-15 ) ) ;
#13286 = EDGE_CURVE ( 'NONE', #22422, #6588, #16431, .T. ) ;
#13287 = AXIS2_PLACEMENT_3D ( 'NONE', #23178, #21051, #15690 ) ;
#13288 = CARTESIAN_POINT ( 'NONE',  ( -8.400427469268855418, 41.24693708775285472, -141.5795910977944061 ) ) ;
#13289 = VECTOR ( 'NONE', #846, 1000.000000000000114 ) ;
#13290 = EDGE_LOOP ( 'NONE', ( #21870, #4748, #12508, #23242 ) ) ;
#13291 = FACE_OUTER_BOUND ( 'NONE', #23309, .T. ) ;
#13292 = ADVANCED_FACE ( 'NONE', ( #19621 ), #18069, .F. ) ;
#13293 = CARTESIAN_POINT ( 'NONE',  ( 10.00000637188149177, 37.10042154059043185, -146.5552973561727583 ) ) ;
#13294 = CARTESIAN_POINT ( 'NONE',  ( -25.64792992860000354, 37.04465132570000208, -139.7265440090000084 ) ) ;
#13295 = EDGE_LOOP ( 'NONE', ( #15428, #4630, #5674, #13845 ) ) ;
#13296 = CARTESIAN_POINT ( 'NONE',  ( -12.98514687064261963, 38.77227581979464333, -147.9931195024429087 ) ) ;
#13297 = DIRECTION ( 'NONE',  ( 1.000000000000000000, -5.094701941669999797E-24, -2.257144641399999941E-12 ) ) ;
#13298 = CARTESIAN_POINT ( 'NONE',  ( 16.29836742280000195, -22.74229684829999698, -142.5552959529999839 ) ) ;
#13299 = ORIENTED_EDGE ( 'NONE', *, *, #18080, .T. ) ;
#13300 = DIRECTION ( 'NONE',  ( -2.257144641399999941E-12, 8.049635416090000264E-35, -1.000000000000000000 ) ) ;
#13301 = DIRECTION ( 'NONE',  ( 0.000000000000000000, 1.000000000000000000, -2.245315044999999693E-12 ) ) ;
#13302 = VECTOR ( 'NONE', #14987, 1000.000000000000000 ) ;
#13303 =( BOUNDED_CURVE ( )  B_SPLINE_CURVE ( 5, ( #22237, #3808, #16878, #7822, #474, #20572 ),
 .UNSPECIFIED., .F., .F. ) 
 B_SPLINE_CURVE_WITH_KNOTS ( ( 6, 6 ),
 ( 1.570796326891506167, 3.141592653590000062 ),
 .UNSPECIFIED. ) 
 CURVE ( )  GEOMETRIC_REPRESENTATION_ITEM ( )  RATIONAL_B_SPLINE_CURVE ( ( 0.2500000000000000000, 0.2500000000122875043, 0.3000000000184313009, 0.4000000000245750864, 0.6000000000245750975, 1.000000000000000000 ) ) 
 REPRESENTATION_ITEM ( '' )  );
#13304 = VECTOR ( 'NONE', #13059, 1000.000000000000000 ) ;
#13305 = ORIENTED_EDGE ( 'NONE', *, *, #19917, .T. ) ;
#13306 = PLANE ( 'NONE',  #5685 ) ;
#13307 = CARTESIAN_POINT ( 'NONE',  ( -2.203055323360000095, -15.74846988260000025, -143.5552959529999839 ) ) ;
#13308 = ORIENTED_EDGE ( 'NONE', *, *, #676, .F. ) ;
#13309 = CARTESIAN_POINT ( 'NONE',  ( -5.101475126953193495, 45.72676979428539568, -150.0552959529999839 ) ) ;
#13310 = EDGE_CURVE ( 'NONE', #10073, #16792, #18184, .T. ) ;
#13311 = CARTESIAN_POINT ( 'NONE',  ( -20.84101097272391812, 38.55092845023212078, -147.7610021333602219 ) ) ;
#13312 = ORIENTED_EDGE ( 'NONE', *, *, #14297, .T. ) ;
#13313 = EDGE_CURVE ( 'NONE', #23177, #19038, #1901, .T. ) ;
#13314 = CARTESIAN_POINT ( 'NONE',  ( -27.23537055383044247, 34.33249971486813479, -147.5370179225575953 ) ) ;
#13315 = CARTESIAN_POINT ( 'NONE',  ( -18.07392865170000107, -34.50000000000000000, -145.5657682190000060 ) ) ;
#13316 = ORIENTED_EDGE ( 'NONE', *, *, #15724, .T. ) ;
#13317 = CYLINDRICAL_SURFACE ( 'NONE', #4139, 2.000000000000001776 ) ;
#13318 = CARTESIAN_POINT ( 'NONE',  ( -35.07300000000000040, 11.44852983560000048, -144.5552959529999839 ) ) ;
#13319 = CARTESIAN_POINT ( 'NONE',  ( -9.971101149720000834, 37.05360750090000721, -147.8421425029999909 ) ) ;
#13320 = ORIENTED_EDGE ( 'NONE', *, *, #21398, .F. ) ;
#13321 = ADVANCED_FACE ( 'NONE', ( #115 ), #5567, .T. ) ;
#13322 = CARTESIAN_POINT ( 'NONE',  ( -21.35824191591069265, -32.00000000000000000, -141.9623572383524959 ) ) ;
#13323 = EDGE_CURVE ( 'NONE', #2700, #12291, #1781, .T. ) ;
#13324 = LINE ( 'NONE', #16782, #13998 ) ;
#13325 = ORIENTED_EDGE ( 'NONE', *, *, #14623, .F. ) ;
#13326 = VECTOR ( 'NONE', #755, 1000.000000000000000 ) ;
#13327 = ADVANCED_FACE ( 'NONE', ( #1552 ), #16168, .F. ) ;
#13328 = ORIENTED_EDGE ( 'NONE', *, *, #7700, .T. ) ;
#13329 = DIRECTION ( 'NONE',  ( 1.000000000000000000, 0.000000000000000000, -2.775557561562892298E-14 ) ) ;
#13330 = CARTESIAN_POINT ( 'NONE',  ( 3.999999999879999546, -3.000000000000000000, -135.4552959529999896 ) ) ;
#13331 = DIRECTION ( 'NONE',  ( 0.000000000000000000, 0.000000000000000000, -1.000000000000000000 ) ) ;
#13332 = DIRECTION ( 'NONE',  ( 2.839308199605699858E-14, 3.568879590633174872E-13, 1.000000000000000000 ) ) ;
#13333 = EDGE_LOOP ( 'NONE', ( #23510, #7817, #6520, #7645 ) ) ;
#13334 = LINE ( 'NONE', #617, #21189 ) ;
#13335 = CARTESIAN_POINT ( 'NONE',  ( 3.611688725869999975E-11, -39.98606797749999942, -136.0552959530000123 ) ) ;
#13336 = FACE_OUTER_BOUND ( 'NONE', #22493, .T. ) ;
#13337 = CARTESIAN_POINT ( 'NONE',  ( -9.347107914279998653, -17.32706600430000066, -143.5552959529999839 ) ) ;
#13338 = CARTESIAN_POINT ( 'NONE',  ( -32.50000000000000000, 26.00000000000000000, -141.5552959529999839 ) ) ;
#13339 = AXIS2_PLACEMENT_3D ( 'NONE', #4734, #8164, #17222 ) ;
#13340 = CLOSED_SHELL ( 'NONE', ( #4891, #665, #10544, #21452, #10527, #14059, #15153, #13292, #5179, #18694, #22768, #14670, #21211, #15936, #22088, #4109, #11223, #2540, #13150, #7327, #9649, #19380, #22044, #9078, #1692, #8655, #17987, #2013, #18333, #9874 ) ) ;
#13341 = VECTOR ( 'NONE', #9086, 1000.000000000000000 ) ;
#13342 = CARTESIAN_POINT ( 'NONE',  ( -15.67014142460604020, 35.45905754580739710, -147.3461856841272208 ) ) ;
#13343 = CARTESIAN_POINT ( 'NONE',  ( -15.94523344347496163, 33.71216531382139436, -145.7766456663748045 ) ) ;
#13344 = DIRECTION ( 'NONE',  ( 2.602084704489999637E-17, -1.000000000000000000, -4.426606872070000353E-37 ) ) ;
#13345 = LINE ( 'NONE', #3962, #21362 ) ;
#13346 = DIRECTION ( 'NONE',  ( 0.000000000000000000, 0.000000000000000000, 1.000000000000000000 ) ) ;
#13347 = ORIENTED_EDGE ( 'NONE', *, *, #2409, .T. ) ;
#13348 = ADVANCED_FACE ( 'NONE', ( #15925, #23192 ), #21414, .T. ) ;
#13349 = CARTESIAN_POINT ( 'NONE',  ( -9.906675138925947977, 36.27859082920983980, -147.4875108566695303 ) ) ;
#13350 = CARTESIAN_POINT ( 'NONE',  ( 25.50000000000000000, 25.50000000000000000, -136.5552959530000123 ) ) ;
#13351 = EDGE_CURVE ( 'NONE', #5909, #22853, #12461, .T. ) ;
#13352 = VERTEX_POINT ( 'NONE', #18309 ) ;
#13353 = CARTESIAN_POINT ( 'NONE',  ( -2.499999999859999988, 31.00000000000000000, -147.5552959529999839 ) ) ;
#13354 = CARTESIAN_POINT ( 'NONE',  ( -22.52056272209999932, 33.27763168300000274, -146.2006519230000094 ) ) ;
#13355 = CIRCLE ( 'NONE', #6904, 2.500000000000002220 ) ;
#13356 = AXIS2_PLACEMENT_3D ( 'NONE', #2074, #4314, #9180 ) ;
#13357 = CARTESIAN_POINT ( 'NONE',  ( 16.61718498210000305, -18.75502267109999721, -143.0552959529999839 ) ) ;
#13358 = ORIENTED_EDGE ( 'NONE', *, *, #2305, .T. ) ;
#13359 = VECTOR ( 'NONE', #11657, 1000.000000000000000 ) ;
#13360 = CARTESIAN_POINT ( 'NONE',  ( -13.47165290135673921, 33.35876621941304165, -143.8174469061277989 ) ) ;
#13361 = DIRECTION ( 'NONE',  ( 2.259525899719999991E-12, 0.000000000000000000, 1.000000000000000000 ) ) ;
#13362 = LINE ( 'NONE', #4327, #5965 ) ;
#13363 = FACE_OUTER_BOUND ( 'NONE', #692, .T. ) ;
#13364 = DIRECTION ( 'NONE',  ( -0.9840552701943220404, 0.1778629393740580045, -3.651917849741195385E-14 ) ) ;
#13365 = CARTESIAN_POINT ( 'NONE',  ( 6.148946002022614543, -33.04517854815976108, -150.0552959529999839 ) ) ;
#13366 = ORIENTED_EDGE ( 'NONE', *, *, #16819, .T. ) ;
#13367 = CARTESIAN_POINT ( 'NONE',  ( -7.500000000000000000, 42.50000000000000000, -151.0552959529999839 ) ) ;
#13368 = ORIENTED_EDGE ( 'NONE', *, *, #11924, .T. ) ;
#13369 = CARTESIAN_POINT ( 'NONE',  ( -13.38748872343123963, 33.38537881997591228, -144.5933708984670147 ) ) ;
#13370 = DIRECTION ( 'NONE',  ( 0.2451800884060535979, 0.9694775522152123681, -1.311492566970288567E-12 ) ) ;
#13371 = CIRCLE ( 'NONE', #2004, 5.999999999999998224 ) ;
#13372 = AXIS2_PLACEMENT_3D ( 'NONE', #4539, #22628, #6318 ) ;
#13373 = CARTESIAN_POINT ( 'NONE',  ( 24.68320006080000084, -24.50000000000000000, -150.0552959529999839 ) ) ;
#13374 = EDGE_CURVE ( 'NONE', #361, #10851, #13375, .T. ) ;
#13375 = CIRCLE ( 'NONE', #3132, 5.000000000000000000 ) ;
#13376 = EDGE_LOOP ( 'NONE', ( #4914, #8652, #16772, #11933, #18229 ) ) ;
#13377 = ADVANCED_FACE ( 'NONE', ( #15198 ), #11032, .T. ) ;
#13378 = DIRECTION ( 'NONE',  ( 8.955190032050000935E-12, -9.104778821549999739E-13, 1.000000000000000000 ) ) ;
#13379 = LINE ( 'NONE', #305, #7595 ) ;
#13380 = EDGE_CURVE ( 'NONE', #30, #21927, #2242, .T. ) ;
#13381 = EDGE_LOOP ( 'NONE', ( #2850, #22874 ) ) ;
#13382 = CARTESIAN_POINT ( 'NONE',  ( -20.21101409811915772, 36.97743810397759745, -140.7155889590012237 ) ) ;
#13383 = CARTESIAN_POINT ( 'NONE',  ( 9.091636166211589654, 38.37840305069799030, -141.9696471534239777 ) ) ;
#13384 = DIRECTION ( 'NONE',  ( 2.257144641399999941E-12, -8.049635416090000264E-35, 1.000000000000000000 ) ) ;
#13385 = CARTESIAN_POINT ( 'NONE',  ( -22.79386933271688420, 37.02723109250344891, -140.7029355817511771 ) ) ;
#13386 = CARTESIAN_POINT ( 'NONE',  ( -25.12153080232964086, 33.08100675563860449, -141.7696838823344194 ) ) ;
#13387 = VERTEX_POINT ( 'NONE', #9348 ) ;
#13388 = CARTESIAN_POINT ( 'NONE',  ( -6.604791614870066496, -20.14156755886077832, -144.5552959529732959 ) ) ;
#13389 = ORIENTED_EDGE ( 'NONE', *, *, #4849, .T. ) ;
#13390 = DIRECTION ( 'NONE',  ( 0.000000000000000000, 0.000000000000000000, 1.000000000000000000 ) ) ;
#13391 = ORIENTED_EDGE ( 'NONE', *, *, #12285, .T. ) ;
#13392 = ORIENTED_EDGE ( 'NONE', *, *, #23355, .F. ) ;
#13393 = CARTESIAN_POINT ( 'NONE',  ( -32.50000000000000000, 50.50000000000000000, -149.5552959529999839 ) ) ;
#13394 = ORIENTED_EDGE ( 'NONE', *, *, #22820, .T. ) ;
#13395 = CARTESIAN_POINT ( 'NONE',  ( 1.000000000140000012, 36.50000000000000000, -147.0552959529999839 ) ) ;
#13396 = EDGE_LOOP ( 'NONE', ( #21796, #10989, #11387, #14946 ) ) ;
#13397 = ORIENTED_EDGE ( 'NONE', *, *, #17026, .F. ) ;
#13398 = EDGE_CURVE ( 'NONE', #21024, #16708, #2477, .T. ) ;
#13399 = CARTESIAN_POINT ( 'NONE',  ( -27.06022691627751797, 38.83733237962867690, -148.2479545111105779 ) ) ;
#13400 = DIRECTION ( 'NONE',  ( 8.955190032050000935E-12, -9.104778821549999739E-13, 1.000000000000000000 ) ) ;
#13401 = LINE ( 'NONE', #8038, #3151 ) ;
#13402 =( GEOMETRIC_REPRESENTATION_CONTEXT ( 3 ) GLOBAL_UNCERTAINTY_ASSIGNED_CONTEXT ( ( #6843 ) ) GLOBAL_UNIT_ASSIGNED_CONTEXT ( ( #16105, #4921, #10135 ) ) REPRESENTATION_CONTEXT ( 'NONE', 'WORKASPACE' ) );
#13403 = ADVANCED_FACE ( 'NONE', ( #688 ), #22223, .F. ) ;
#13404 = CARTESIAN_POINT ( 'NONE',  ( -11.85909339612901015, 36.92087135289245481, -147.9691652863633067 ) ) ;
#13405 = DIRECTION ( 'NONE',  ( -1.000000000000000000, 0.000000000000000000, -2.508215857230000030E-12 ) ) ;
#13406 = EDGE_LOOP ( 'NONE', ( #23280, #13533, #16200, #8398 ) ) ;
#13407 = CARTESIAN_POINT ( 'NONE',  ( -9.347107914279998653, -17.32706600430000066, -143.5552959529999839 ) ) ;
#13408 = CARTESIAN_POINT ( 'NONE',  ( -13.92432874550000044, 37.01165864720000087, -139.5650670249999905 ) ) ;
#13409 = EDGE_CURVE ( 'NONE', #2618, #1486, #456, .T. ) ;
#13410 = CARTESIAN_POINT ( 'NONE',  ( 4.109416060118438629, -2.038050104594628653, -136.0552959530093062 ) ) ;
#13411 = ORIENTED_EDGE ( 'NONE', *, *, #10863, .T. ) ;
#13412 = DIRECTION ( 'NONE',  ( 0.09606172499277226828, 0.9953753789357124848, -8.277822871607614780E-13 ) ) ;
#13413 = PLANE ( 'NONE',  #753 ) ;
#13414 = ORIENTED_EDGE ( 'NONE', *, *, #854, .F. ) ;
#13415 = CARTESIAN_POINT ( 'NONE',  ( 17.06104532839999877, -32.02344838739999489, -142.5552959529999839 ) ) ;
#13416 = PRODUCT_DEFINITION_FORMATION_WITH_SPECIFIED_SOURCE ( 'ANY', '', #15507, .NOT_KNOWN. ) ;
#13417 = CARTESIAN_POINT ( 'NONE',  ( 0.5000000001409999895, 20.50000000000000000, -147.5552959529999839 ) ) ;
#13418 = ADVANCED_FACE ( 'NONE', ( #6028 ), #16743, .T. ) ;
#13419 = ORIENTED_EDGE ( 'NONE', *, *, #12914, .F. ) ;
#13420 = CARTESIAN_POINT ( 'NONE',  ( 4.500000000009999113, -3.500000000000000000, -137.0552959530000123 ) ) ;
#13421 = CARTESIAN_POINT ( 'NONE',  ( 20.50000000000000000, 25.50000000000000000, -150.5552959529999839 ) ) ;
#13422 = ORIENTED_EDGE ( 'NONE', *, *, #16103, .T. ) ;
#13423 = CARTESIAN_POINT ( 'NONE',  ( -4.510096969224879793, 46.24633263602949995, -150.0552959529999839 ) ) ;
#13424 = CARTESIAN_POINT ( 'NONE',  ( -20.76253627919999900, 39.57534689110000414, -140.5049880910000013 ) ) ;
#13425 = EDGE_LOOP ( 'NONE', ( #705, #7669, #13161, #15354 ) ) ;
#13426 = CARTESIAN_POINT ( 'NONE',  ( -27.65087262191089224, 32.98947248583699832, -143.4940380741495289 ) ) ;
#13427 = DIRECTION ( 'NONE',  ( -5.094701932209999624E-24, -1.000000000000000000, 1.149947916579999802E-35 ) ) ;
#13428 = VERTEX_POINT ( 'NONE', #7918 ) ;
#13429 = CARTESIAN_POINT ( 'NONE',  ( 3.249999999879999990, -3.000000000000000000, -135.0552959530000123 ) ) ;
#13430 = DIRECTION ( 'NONE',  ( 1.000000000000000000, 0.000000000000000000, 0.000000000000000000 ) ) ;
#13431 = VERTEX_POINT ( 'NONE', #7462 ) ;
#13432 = EDGE_CURVE ( 'NONE', #16041, #15836, #5912, .T. ) ;
#13433 = CARTESIAN_POINT ( 'NONE',  ( -21.35824191589999899, -32.00000000000000000, -146.3157682190000060 ) ) ;
#13434 = VERTEX_POINT ( 'NONE', #12817 ) ;
#13435 = CARTESIAN_POINT ( 'NONE',  ( -8.514310886080000529, 36.94123471670000214, -140.1199228270000106 ) ) ;
#13436 = DIRECTION ( 'NONE',  ( -2.257144641399999941E-12, 0.000000000000000000, -1.000000000000000000 ) ) ;
#13437 = ORIENTED_EDGE ( 'NONE', *, *, #7805, .T. ) ;
#13438 = EDGE_CURVE ( 'NONE', #10143, #3905, #4129, .T. ) ;
#13439 = ORIENTED_EDGE ( 'NONE', *, *, #7628, .F. ) ;
#13440 = SHAPE_REPRESENTATION ( 'Latch Lever Guide', ( #5025 ), #21773 ) ;
#13441 = CARTESIAN_POINT ( 'NONE',  ( 6.010856941112696639, -0.8786408349372250015, -150.0552959529999839 ) ) ;
#13442 = CARTESIAN_POINT ( 'NONE',  ( -30.28539838652671179, 40.31549301428387366, -145.3075639834989090 ) ) ;
#13443 = CARTESIAN_POINT ( 'NONE',  ( -13.92432874550000044, 37.01165864720000087, -139.5650670249999905 ) ) ;
#13444 = CARTESIAN_POINT ( 'NONE',  ( 12.90429904045548426, -17.98118184282727938, -144.5552959530160422 ) ) ;
#13445 = ORIENTED_EDGE ( 'NONE', *, *, #22979, .T. ) ;
#13446 = CARTESIAN_POINT ( 'NONE',  ( 31.49999999989999822, 32.96379895120000469, -136.0552959530000123 ) ) ;
#13447 = DIRECTION ( 'NONE',  ( 1.000000000000000000, 2.602084704489999637E-17, -1.701177084980000217E-20 ) ) ;
#13448 = EDGE_CURVE ( 'NONE', #3522, #1160, #17182, .T. ) ;
#13449 = CARTESIAN_POINT ( 'NONE',  ( -14.08011361694696539, -41.79914019397068614, -150.0552959529999839 ) ) ;
#13450 = LINE ( 'NONE', #13564, #20588 ) ;
#13451 = CARTESIAN_POINT ( 'NONE',  ( 1.759100530420000030, -16.38142836440000139, -143.5552959529999839 ) ) ;
#13452 = EDGE_CURVE ( 'NONE', #8634, #20086, #3791, .T. ) ;
#13453 = CARTESIAN_POINT ( 'NONE',  ( 10.06924771219168235, -19.69968182150093128, -148.5552959529999839 ) ) ;
#13454 = EDGE_CURVE ( 'NONE', #17813, #14322, #18802, .T. ) ;
#13455 = CIRCLE ( 'NONE', #10015, 15.00000000000000178 ) ;
#13456 = CARTESIAN_POINT ( 'NONE',  ( 4.499999999879999102, -3.500000000000000000, -143.0552959529999839 ) ) ;
#13457 = EDGE_CURVE ( 'NONE', #11758, #22236, #13057, .T. ) ;
#13458 = DIRECTION ( 'NONE',  ( 0.000000000000000000, -1.000000000000000000, -2.602084704489999637E-17 ) ) ;
#13459 = PLANE ( 'NONE',  #13372 ) ;
#13460 = DIRECTION ( 'NONE',  ( 0.000000000000000000, 1.000000000000000000, 0.000000000000000000 ) ) ;
#13461 = ORIENTED_EDGE ( 'NONE', *, *, #1180, .T. ) ;
#13462 = CARTESIAN_POINT ( 'NONE',  ( -9.801780389369936231, 37.03339632395869074, -147.4803110669174657 ) ) ;
#13463 = CARTESIAN_POINT ( 'NONE',  ( 32.50000000000000000, -21.03620104879999886, -137.0552959530000123 ) ) ;
#13464 = CARTESIAN_POINT ( 'NONE',  ( -36.49999999989999822, 37.00000000000000000, -138.5552959529999839 ) ) ;
#13465 = EDGE_LOOP ( 'NONE', ( #10766, #18853, #9205, #18763 ) ) ;
#13466 = DIRECTION ( 'NONE',  ( -1.211690350419999855E-27, -2.765629237170000203E-27, 1.000000000000000000 ) ) ;
#13467 = CARTESIAN_POINT ( 'NONE',  ( -22.75008518894089704, 33.18911177007243651, -144.4560875053247457 ) ) ;
#13468 = CARTESIAN_POINT ( 'NONE',  ( -9.282104535860000283, -16.71402168319999859, -145.5552959529999839 ) ) ;
#13469 = ORIENTED_EDGE ( 'NONE', *, *, #19383, .F. ) ;
#13470 = ADVANCED_FACE ( 'NONE', ( #19356 ), #8401, .F. ) ;
#13471 = LINE ( 'NONE', #762, #15042 ) ;
#13472 = CARTESIAN_POINT ( 'NONE',  ( -35.73252798949999942, 26.50000000000000000, -140.5552959529999839 ) ) ;
#13473 = LINE ( 'NONE', #3021, #6798 ) ;
#13474 = DIRECTION ( 'NONE',  ( 1.000000000000000000, -5.094701941669999797E-24, -2.257144641399999941E-12 ) ) ;
#13475 = CARTESIAN_POINT ( 'NONE',  ( -32.50000000000000000, 0.9999999999959999775, -155.5552959529999839 ) ) ;
#13476 = CARTESIAN_POINT ( 'NONE',  ( -8.810109936767679173, 39.32487244797151504, -140.7337397743969802 ) ) ;
#13477 = ORIENTED_EDGE ( 'NONE', *, *, #12296, .F. ) ;
#13478 = EDGE_CURVE ( 'NONE', #7389, #17215, #4605, .T. ) ;
#13479 = CARTESIAN_POINT ( 'NONE',  ( -28.32050416868494125, 34.28824206719405510, -147.8072173032999217 ) ) ;
#13480 =( NAMED_UNIT ( * ) PLANE_ANGLE_UNIT ( ) SI_UNIT ( $, .RADIAN. ) );
#13481 = ORIENTED_EDGE ( 'NONE', *, *, #22414, .F. ) ;
#13482 = CARTESIAN_POINT ( 'NONE',  ( -14.39443208618090253, 34.43246107294096703, -140.8168812543075603 ) ) ;
#13483 = ADVANCED_FACE ( 'NONE', ( #4838 ), #10050, .T. ) ;
#13484 = DIRECTION ( 'NONE',  ( -1.000000000000000000, 0.000000000000000000, 0.000000000000000000 ) ) ;
#13485 = CARTESIAN_POINT ( 'NONE',  ( 32.50000000000000000, -21.03620104879999886, -136.0552959530000123 ) ) ;
#13486 = ORIENTED_EDGE ( 'NONE', *, *, #16428, .F. ) ;
#13487 = PLANE ( 'NONE',  #21672 ) ;
#13488 = CARTESIAN_POINT ( 'NONE',  ( 7.000000000060000005, 37.00000000000000000, -142.5552959529999839 ) ) ;
#13489 = AXIS2_PLACEMENT_3D ( 'NONE', #11294, #18921, #20710 ) ;
#13490 = ORIENTED_EDGE ( 'NONE', *, *, #21142, .F. ) ;
#13491 = LINE ( 'NONE', #10027, #18647 ) ;
#13492 = CARTESIAN_POINT ( 'NONE',  ( -18.27025349466079973, 40.59684088653609280, -144.3213525969109128 ) ) ;
#13493 = CARTESIAN_POINT ( 'NONE',  ( 7.746249104743133884, 38.30079617153757710, -146.1911047861169379 ) ) ;
#13494 = DIRECTION ( 'NONE',  ( 2.257252162960000001E-12, 0.000000000000000000, 1.000000000000000000 ) ) ;
#13495 = CARTESIAN_POINT ( 'NONE',  ( -24.56649898262948994, 33.80095595918812990, -145.8672865390101663 ) ) ;
#13496 = CARTESIAN_POINT ( 'NONE',  ( 3.299235031439282650, -4.419791545611266415, -150.0552959529999555 ) ) ;
#13497 = ORIENTED_EDGE ( 'NONE', *, *, #17535, .T. ) ;
#13498 = ADVANCED_FACE ( 'NONE', ( #9938 ), #12082, .F. ) ;
#13499 = LINE ( 'NONE', #15059, #19454 ) ;
#13500 = EDGE_LOOP ( 'NONE', ( #11637, #10385, #10558, #16101 ) ) ;
#13501 = VECTOR ( 'NONE', #13690, 1000.000000000000000 ) ;
#13502 = DIRECTION ( 'NONE',  ( -1.527666881879999979E-13, -8.171241461240000022E-13, -1.000000000000000000 ) ) ;
#13503 = AXIS2_PLACEMENT_3D ( 'NONE', #8601, #11942, #6597 ) ;
#13504 = VERTEX_POINT ( 'NONE', #15424 ) ;
#13505 = CARTESIAN_POINT ( 'NONE',  ( -26.76912629117864739, 37.72282967552698807, -147.8698271774196371 ) ) ;
#13506 = ORIENTED_EDGE ( 'NONE', *, *, #15168, .T. ) ;
#13507 = DIRECTION ( 'NONE',  ( -0.1146332952500066227, -0.9934078757590583120, -9.663381206340560633E-14 ) ) ;
#13508 = ORIENTED_EDGE ( 'NONE', *, *, #23330, .F. ) ;
#13509 = CARTESIAN_POINT ( 'NONE',  ( -30.49999999990000177, 45.00000000000000000, -140.5552959529999839 ) ) ;
#13510 = ORIENTED_EDGE ( 'NONE', *, *, #4952, .T. ) ;
#13511 = ORIENTED_EDGE ( 'NONE', *, *, #16368, .F. ) ;
#13512 = LINE ( 'NONE', #15542, #10991 ) ;
#13513 = DIRECTION ( 'NONE',  ( 0.000000000000000000, 1.000000000000000000, 0.000000000000000000 ) ) ;
#13514 = CARTESIAN_POINT ( 'NONE',  ( -10.51976837306068191, 37.87277224112855123, -140.3566920414173467 ) ) ;
#13515 = FILL_AREA_STYLE_COLOUR ( '', #7419 ) ;
#13516 = LINE ( 'NONE', #20440, #7615 ) ;
#13517 = B_SPLINE_CURVE_WITH_KNOTS ( 'NONE', 3,
 ( #1044, #2713, #15425, #1292, #2942, #13880 ),
 .UNSPECIFIED., .F., .F.,
 ( 4, 2, 4 ),
 ( 0.000000000000000000, 0.5000000000000000000, 1.000000000000000000 ),
 .UNSPECIFIED. ) ;
#13518 = CARTESIAN_POINT ( 'NONE',  ( -9.562013113444260526, 37.00477621355918245, -148.7272342975820436 ) ) ;
#13519 = ORIENTED_EDGE ( 'NONE', *, *, #3474, .T. ) ;
#13520 = LINE ( 'NONE', #20793, #23522 ) ;
#13521 = VECTOR ( 'NONE', #7229, 1000.000000000000114 ) ;
#13522 = VECTOR ( 'NONE', #5031, 1000.000000000000000 ) ;
#13523 = CARTESIAN_POINT ( 'NONE',  ( 27.18320006080000084, 0.9999999999989999111, -150.0552959529999839 ) ) ;
#13524 = CARTESIAN_POINT ( 'NONE',  ( 25.11919234682703461, 34.98537695657089586, -150.0552959529999839 ) ) ;
#13525 = EDGE_LOOP ( 'NONE', ( #15657, #15004, #14911, #22358, #6849, #18177 ) ) ;
#13526 = EDGE_CURVE ( 'NONE', #7124, #18273, #13401, .T. ) ;
#13527 = CARTESIAN_POINT ( 'NONE',  ( -18.05676631878100125, 41.24287485562951616, -146.4171244423180838 ) ) ;
#13528 = CARTESIAN_POINT ( 'NONE',  ( 23.50000000000000000, -20.50000000000000000, -137.0552959530000123 ) ) ;
#13529 = VERTEX_POINT ( 'NONE', #22574 ) ;
#13530 =( LENGTH_UNIT ( ) NAMED_UNIT ( * ) SI_UNIT ( .MILLI., .METRE. ) );
#13531 = EDGE_CURVE ( 'NONE', #5806, #21392, #22919, .T. ) ;
#13532 = PLANE ( 'NONE',  #13132 ) ;
#13533 = ORIENTED_EDGE ( 'NONE', *, *, #6555, .F. ) ;
#13534 = DIRECTION ( 'NONE',  ( 7.389987738588579788E-14, 0.000000000000000000, 1.000000000000000000 ) ) ;
#13535 = CARTESIAN_POINT ( 'NONE',  ( 23.89269908169873702, -23.49999999999999645, -150.0552959529999839 ) ) ;
#13536 = VERTEX_POINT ( 'NONE', #17445 ) ;
#13537 =( BOUNDED_CURVE ( )  B_SPLINE_CURVE ( 5, ( #15077, #9246, #7463, #18310, #20438, #11490 ),
 .UNSPECIFIED., .F., .F. ) 
 B_SPLINE_CURVE_WITH_KNOTS ( ( 6, 6 ),
 ( 1.570796326505558893, 3.141592653590000062 ),
 .UNSPECIFIED. ) 
 CURVE ( )  GEOMETRIC_REPRESENTATION_ITEM ( )  RATIONAL_B_SPLINE_CURVE ( ( 0.2500000000000000000, 0.2499999999631472292, 0.2999999999447208188, 0.3999999999262944250, 0.5999999999262943806, 1.000000000000000000 ) ) 
 REPRESENTATION_ITEM ( '' )  );
#13538 = CARTESIAN_POINT ( 'NONE',  ( -14.58162373618102059, 40.18882273014816064, -142.1871799655052087 ) ) ;
#13539 = VECTOR ( 'NONE', #20828, 1000.000000000000000 ) ;
#13540 = CARTESIAN_POINT ( 'NONE',  ( -24.26662447743907691, 35.20109951642859869, -148.0073960929780128 ) ) ;
#13541 = EDGE_LOOP ( 'NONE', ( #17338, #1553, #14675, #4497 ) ) ;
#13542 = CARTESIAN_POINT ( 'NONE',  ( -32.50000000000000000, 21.50000000000000000, -137.0552959530000123 ) ) ;
#13543 = ORIENTED_EDGE ( 'NONE', *, *, #5693, .T. ) ;
#13544 = CARTESIAN_POINT ( 'NONE',  ( 2.500000000170000014, 24.50000000000000000, -136.5552959530000123 ) ) ;
#13545 = CARTESIAN_POINT ( 'NONE',  ( -7.499999999969999109, 48.50000000000000000, -136.5552959530000123 ) ) ;
#13546 = ORIENTED_EDGE ( 'NONE', *, *, #10626, .F. ) ;
#13547 = CARTESIAN_POINT ( 'NONE',  ( -9.282104535849999394, -16.71402168319999859, -144.5552959529999839 ) ) ;
#13548 = ADVANCED_FACE ( 'NONE', ( #13879 ), #20914, .T. ) ;
#13549 = EDGE_LOOP ( 'NONE', ( #6326, #12229, #6643 ) ) ;
#13550 = DIRECTION ( 'NONE',  ( 0.000000000000000000, 1.000000000000000000, 0.000000000000000000 ) ) ;
#13551 = DIRECTION ( 'NONE',  ( 2.602084747549999882E-17, -1.000000000000000000, -5.873289694040000105E-29 ) ) ;
#13552 = ORIENTED_EDGE ( 'NONE', *, *, #5882, .T. ) ;
#13553 = ADVANCED_FACE ( 'NONE', ( #1171 ), #20752, .F. ) ;
#13554 = AXIS2_PLACEMENT_3D ( 'NONE', #7252, #19753, #6771 ) ;
#13555 = VERTEX_POINT ( 'NONE', #19483 ) ;
#13556 = FACE_OUTER_BOUND ( 'NONE', #1840, .T. ) ;
#13557 = CARTESIAN_POINT ( 'NONE',  ( -12.50000000000000000, 19.50000000000000000, -150.5552959529999839 ) ) ;
#13558 = DIRECTION ( 'NONE',  ( 1.000000000000000000, 2.602084704489999637E-17, -2.257171095940000041E-12 ) ) ;
#13559 = DIRECTION ( 'NONE',  ( -8.955503005839999404E-12, 9.094947017729999296E-13, -1.000000000000000000 ) ) ;
#13560 = ORIENTED_EDGE ( 'NONE', *, *, #18092, .F. ) ;
#13561 = EDGE_CURVE ( 'NONE', #7005, #23370, #8743, .T. ) ;
#13562 = CARTESIAN_POINT ( 'NONE',  ( -7.728596210859999260, 38.74386132360000090, -140.2295773360000055 ) ) ;
#13563 = CARTESIAN_POINT ( 'NONE',  ( 31.50000000000000000, 20.96379895120000114, -137.0552959530000123 ) ) ;
#13564 = CARTESIAN_POINT ( 'NONE',  ( 0.000000000000000000, 47.50000000000000000, -150.0552959529999839 ) ) ;
#13565 = LINE ( 'NONE', #8450, #7539 ) ;
#13566 = ORIENTED_EDGE ( 'NONE', *, *, #3278, .F. ) ;
#13567 = CARTESIAN_POINT ( 'NONE',  ( -16.71251657190000017, 33.01037093000000766, -141.5651630139999781 ) ) ;
#13568 = CIRCLE ( 'NONE', #1828, 15.00000000000000178 ) ;
#13569 = CARTESIAN_POINT ( 'NONE',  ( -15.76532943033608092, 34.76918918225535293, -146.9254579970084080 ) ) ;
#13570 = ADVANCED_FACE ( 'NONE', ( #12207 ), #3402, .T. ) ;
#13571 = CARTESIAN_POINT ( 'NONE',  ( -4.584402860569999127, 37.05223431090000474, -140.2914745300000163 ) ) ;
#13572 = LINE ( 'NONE', #19058, #20240 ) ;
#13573 = CARTESIAN_POINT ( 'NONE',  ( 4.500000000009999113, -3.500000000000000000, -137.0552959530000123 ) ) ;
#13574 = ORIENTED_EDGE ( 'NONE', *, *, #8809, .F. ) ;
#13575 = CARTESIAN_POINT ( 'NONE',  ( -10.15741051819999896, 33.19655140199999721, -141.5761258080000005 ) ) ;
#13576 = DIRECTION ( 'NONE',  ( -1.526468026909999897E-13, -8.159623473500000156E-13, -1.000000000000000000 ) ) ;
#13577 = APPLICATION_CONTEXT ( 'automotive_design' ) ;
#13578 = FACE_OUTER_BOUND ( 'NONE', #19155, .T. ) ;
#13579 = EDGE_LOOP ( 'NONE', ( #14145, #11415, #12544, #17928 ) ) ;
#13580 = CARTESIAN_POINT ( 'NONE',  ( -14.47770030809999930, -1.500000000000000000, -147.5552959529999839 ) ) ;
#13581 = EDGE_CURVE ( 'NONE', #73, #3899, #12553, .T. ) ;
#13582 = ADVANCED_FACE ( 'NONE', ( #17686 ), #16260, .F. ) ;
#13583 = CARTESIAN_POINT ( 'NONE',  ( 11.53320006080000049, -24.50000000000000000, -148.5552959529999839 ) ) ;
#13584 = DIRECTION ( 'NONE',  ( -1.000000000000000000, 0.000000000000000000, 0.000000000000000000 ) ) ;
#13585 = VERTEX_POINT ( 'NONE', #17800 ) ;
#13586 = CARTESIAN_POINT ( 'NONE',  ( -23.34997301947807813, 41.23575095046039962, -144.6233831889099974 ) ) ;
#13587 = EDGE_CURVE ( 'NONE', #3235, #4355, #14238, .T. ) ;
#13588 = AXIS2_PLACEMENT_3D ( 'NONE', #3247, #10600, #23356 ) ;
#13589 = DIRECTION ( 'NONE',  ( 0.000000000000000000, 1.000000000000000000, 0.000000000000000000 ) ) ;
#13590 = ADVANCED_FACE ( 'NONE', ( #4544 ), #2536, .F. ) ;
#13591 = CARTESIAN_POINT ( 'NONE',  ( -14.84561440076392813, 36.91926241633399997, -147.9647079511927643 ) ) ;
#13592 = CARTESIAN_POINT ( 'NONE',  ( 31.50000000000000000, 32.96379895120000469, -143.0552959529999839 ) ) ;
#13593 = AXIS2_PLACEMENT_3D ( 'NONE', #10413, #16023, #19596 ) ;
#13594 = CARTESIAN_POINT ( 'NONE',  ( -10.16983759159231049, 35.05179278799776199, -148.3304041598011622 ) ) ;
#13595 = CARTESIAN_POINT ( 'NONE',  ( 7.750000000030000002, -39.98606797749999942, -136.0552959530000123 ) ) ;
#13596 = CARTESIAN_POINT ( 'NONE',  ( 8.750000000000000000, -38.23606797749999942, -150.0552959529999839 ) ) ;
#13597 = PRODUCT ( 'MAS-159', 'MAS-159', '', ( #17763 ) ) ;
#13598 = ORIENTED_EDGE ( 'NONE', *, *, #1834, .T. ) ;
#13599 =( LENGTH_UNIT ( ) NAMED_UNIT ( * ) SI_UNIT ( .MILLI., .METRE. ) );
#13600 = EDGE_LOOP ( 'NONE', ( #6276, #20778, #8567, #10064 ) ) ;
#13601 = EDGE_CURVE ( 'NONE', #16321, #16896, #22632, .T. ) ;
#13602 = CARTESIAN_POINT ( 'NONE',  ( -13.60030749279999895, 34.19157895370000233, -140.3499153360000093 ) ) ;
#13603 = DIRECTION ( 'NONE',  ( 1.000000000000000000, 0.000000000000000000, 0.000000000000000000 ) ) ;
#13604 = DIRECTION ( 'NONE',  ( 1.000000000000000000, 0.000000000000000000, -8.953948693601887499E-12 ) ) ;
#13605 = VECTOR ( 'NONE', #11636, 1000.000000000000227 ) ;
#13606 = EDGE_LOOP ( 'NONE', ( #23040, #15984, #12983 ) ) ;
#13607 = DIRECTION ( 'NONE',  ( 2.257171095940000041E-12, 1.003664318210000046E-28, 1.000000000000000000 ) ) ;
#13608 = PLANE ( 'NONE',  #6076 ) ;
#13609 = CIRCLE ( 'NONE', #15903, 5.999999999999998224 ) ;
#13610 = ORIENTED_EDGE ( 'NONE', *, *, #13286, .F. ) ;
#13611 = CARTESIAN_POINT ( 'NONE',  ( -21.03694116381500123, 36.94210036639135808, -147.9486865822096036 ) ) ;
#13612 = EDGE_CURVE ( 'NONE', #5107, #15057, #11438, .T. ) ;
#13613 = CARTESIAN_POINT ( 'NONE',  ( -18.70477357766290183, 38.50421286460694148, -147.2749284916807824 ) ) ;
#13614 = EDGE_CURVE ( 'NONE', #4947, #22537, #4672, .T. ) ;
#13615 = FACE_BOUND ( 'NONE', #5423, .T. ) ;
#13616 = EDGE_CURVE ( 'NONE', #9607, #1863, #16808, .T. ) ;
#13617 = PLANE ( 'NONE',  #4027 ) ;
#13618 = CARTESIAN_POINT ( 'NONE',  ( -25.60593271316125197, 35.60614443581115296, -140.8684412788813063 ) ) ;
#13619 = CARTESIAN_POINT ( 'NONE',  ( 6.500000000030000002, 20.50000000000000000, -137.0552959530000123 ) ) ;
#13620 = AXIS2_PLACEMENT_3D ( 'NONE', #17581, #8518, #4843 ) ;
#13621 = AXIS2_PLACEMENT_3D ( 'NONE', #8909, #18788, #6057 ) ;
#13622 = EDGE_LOOP ( 'NONE', ( #17322, #549, #3300, #20667 ) ) ;
#13623 = DIRECTION ( 'NONE',  ( 1.000000000000000000, 0.000000000000000000, 0.000000000000000000 ) ) ;
#13624 = AXIS2_PLACEMENT_3D ( 'NONE', #1970, #11203, #5748 ) ;
#13625 = ORIENTED_EDGE ( 'NONE', *, *, #13867, .T. ) ;
#13626 = CARTESIAN_POINT ( 'NONE',  ( -7.499999999959999997, 48.50000000000000000, -136.0552959530000123 ) ) ;
#13627 = ORIENTED_EDGE ( 'NONE', *, *, #2275, .T. ) ;
#13628 = VECTOR ( 'NONE', #2854, 1000.000000000000000 ) ;
#13629 = DIRECTION ( 'NONE',  ( 1.000000000000000000, 0.000000000000000000, -2.775557561562891351E-14 ) ) ;
#13630 = VERTEX_POINT ( 'NONE', #16920 ) ;
#13631 = DIRECTION ( 'NONE',  ( 0.000000000000000000, 2.256988247090000272E-12, 1.000000000000000000 ) ) ;
#13632 = ORIENTED_EDGE ( 'NONE', *, *, #18857, .T. ) ;
#13633 = ORIENTED_EDGE ( 'NONE', *, *, #16653, .F. ) ;
#13634 = CARTESIAN_POINT ( 'NONE',  ( 31.96891336339999867, -40.94938100019999894, -150.0552959529999839 ) ) ;
#13635 = DIRECTION ( 'NONE',  ( 1.000000000000000000, 0.000000000000000000, -2.259303855112193156E-12 ) ) ;
#13636 = DIRECTION ( 'NONE',  ( 2.257144641399999941E-12, 0.000000000000000000, 1.000000000000000000 ) ) ;
#13637 = DIRECTION ( 'NONE',  ( -0.1146332952500066227, -0.9934078757590583120, -9.663381206340560633E-14 ) ) ;
#13638 = DIRECTION ( 'NONE',  ( -2.508215857230000030E-12, 0.000000000000000000, 1.000000000000000000 ) ) ;
#13639 = VECTOR ( 'NONE', #21945, 1000.000000000000000 ) ;
#13640 = EDGE_CURVE ( 'NONE', #4521, #844, #18824, .T. ) ;
#13641 = CARTESIAN_POINT ( 'NONE',  ( 6.500000000159999125, 20.50000000000000000, -139.5552959529999839 ) ) ;
#13642 = EDGE_LOOP ( 'NONE', ( #5531, #12556, #1311, #22100 ) ) ;
#13643 = AXIS2_PLACEMENT_3D ( 'NONE', #4357, #8393, #13629 ) ;
#13644 = CARTESIAN_POINT ( 'NONE',  ( 6.500000000000000000, 28.00000000000000000, -150.5552959529999839 ) ) ;
#13645 = EDGE_CURVE ( 'NONE', #7133, #2000, #17034, .T. ) ;
#13646 = AXIS2_PLACEMENT_3D ( 'NONE', #4508, #11517, #6182 ) ;
#13647 = CARTESIAN_POINT ( 'NONE',  ( 9.841496975946453674, 36.32698089522023821, -146.4634108040735896 ) ) ;
#13648 = VECTOR ( 'NONE', #15283, 1000.000000000000000 ) ;
#13649 = CARTESIAN_POINT ( 'NONE',  ( 24.90181682661750173, 34.66060904161302147, -150.0552959529999839 ) ) ;
#13650 = VERTEX_POINT ( 'NONE', #20729 ) ;
#13651 = CARTESIAN_POINT ( 'NONE',  ( -18.85469010170000459, 37.03971195569999963, -148.4264296979999926 ) ) ;
#13652 = CYLINDRICAL_SURFACE ( 'NONE', #5369, 8.000000000000000000 ) ;
#13653 = ORIENTED_EDGE ( 'NONE', *, *, #1484, .T. ) ;
#13654 = DIRECTION ( 'NONE',  ( -2.257144641399999941E-12, 8.049635416090000264E-35, -1.000000000000000000 ) ) ;
#13655 = AXIS2_PLACEMENT_3D ( 'NONE', #169, #282, #5629 ) ;
#13656 = VERTEX_POINT ( 'NONE', #7866 ) ;
#13657 = CARTESIAN_POINT ( 'NONE',  ( -22.07763076355694665, 37.06632353693416349, -147.8362371614679489 ) ) ;
#13658 = DIRECTION ( 'NONE',  ( -2.507771768019999718E-12, 0.000000000000000000, 1.000000000000000000 ) ) ;
#13659 = ORIENTED_EDGE ( 'NONE', *, *, #2438, .T. ) ;
#13660 = CARTESIAN_POINT ( 'NONE',  ( -15.10539350069024067, 40.90753194052741293, -141.7004951165038449 ) ) ;
#13661 = VECTOR ( 'NONE', #4405, 1000.000000000000000 ) ;
#13662 = CARTESIAN_POINT ( 'NONE',  ( -26.33255611194164558, 36.96293009473756541, -139.4434112040622153 ) ) ;
#13663 = VERTEX_POINT ( 'NONE', #7985 ) ;
#13664 =( LENGTH_UNIT ( ) NAMED_UNIT ( * ) SI_UNIT ( .MILLI., .METRE. ) );
#13665 = VECTOR ( 'NONE', #6262, 999.9999999999998863 ) ;
#13666 = DIRECTION ( 'NONE',  ( -1.000000000000000000, 5.094701932209999624E-24, 0.000000000000000000 ) ) ;
#13667 = ORIENTED_EDGE ( 'NONE', *, *, #13374, .F. ) ;
#13668 = AXIS2_PLACEMENT_3D ( 'NONE', #1330, #8907, #6900 ) ;
#13669 = CARTESIAN_POINT ( 'NONE',  ( -2.500000000000000000, 40.00000000000000000, -150.5552959529999839 ) ) ;
#13670 = DIRECTION ( 'NONE',  ( 8.740345284041279692E-14, 0.000000000000000000, 1.000000000000000000 ) ) ;
#13671 = ORIENTED_EDGE ( 'NONE', *, *, #2044, .T. ) ;
#13672 = DIRECTION ( 'NONE',  ( 1.000000000000000000, 0.000000000000000000, -4.511206223393553012E-12 ) ) ;
#13673 = EDGE_LOOP ( 'NONE', ( #4119, #5493, #15218, #9322, #16346, #19582 ) ) ;
#13674 = EDGE_CURVE ( 'NONE', #7230, #23083, #14910, .T. ) ;
#13675 = LINE ( 'NONE', #20949, #1121 ) ;
#13676 = DIRECTION ( 'NONE',  ( 0.000000000000000000, 0.000000000000000000, 1.000000000000000000 ) ) ;
#13677 = EDGE_CURVE ( 'NONE', #22537, #320, #6177, .T. ) ;
#13678 = ORIENTED_EDGE ( 'NONE', *, *, #12119, .T. ) ;
#13679 = B_SPLINE_CURVE_WITH_KNOTS ( 'NONE', 3,
 ( #18712, #270, #11193, #15256, #5735, #13453, #9289, #16679, #20266, #4415 ),
 .UNSPECIFIED., .F., .F.,
 ( 4, 2, 2, 2, 4 ),
 ( 0.000000000000000000, 0.2500000000000000000, 0.5000000000000000000, 0.7500000000000000000, 1.000000000000000000 ),
 .UNSPECIFIED. ) ;
#13680 = ORIENTED_EDGE ( 'NONE', *, *, #16949, .F. ) ;
#13681 = CIRCLE ( 'NONE', #13283, 5.000000000000000888 ) ;
#13682 = VECTOR ( 'NONE', #7433, 1000.000000000000114 ) ;
#13683 = DIRECTION ( 'NONE',  ( 8.955190032050000935E-12, -9.104778821549999739E-13, 1.000000000000000000 ) ) ;
#13684 = FACE_OUTER_BOUND ( 'NONE', #13210, .T. ) ;
#13685 = VECTOR ( 'NONE', #21383, 1000.000000000000000 ) ;
#13686 = DIRECTION ( 'NONE',  ( 1.000000000000000000, 0.000000000000000000, -4.429789868254373788E-12 ) ) ;
#13687 = DIRECTION ( 'NONE',  ( -2.602084747549999882E-17, 1.000000000000000000, 5.873289694040000105E-29 ) ) ;
#13688 = ORIENTED_EDGE ( 'NONE', *, *, #20975, .F. ) ;
#13689 = CARTESIAN_POINT ( 'NONE',  ( -16.50000000000000000, -43.00000000000000000, -136.0552959530000123 ) ) ;
#13690 = DIRECTION ( 'NONE',  ( 0.000000000000000000, 1.000000000000000000, 0.000000000000000000 ) ) ;
#13691 = DIRECTION ( 'NONE',  ( -1.000000000000000000, 0.000000000000000000, 0.000000000000000000 ) ) ;
#13692 = DIRECTION ( 'NONE',  ( -4.430233957459999899E-12, 6.110667527539999876E-13, -1.000000000000000000 ) ) ;
#13693 = CARTESIAN_POINT ( 'NONE',  ( 23.78818517497825269, -17.51387386319285611, -142.5552959530024566 ) ) ;
#13694 = CARTESIAN_POINT ( 'NONE',  ( 3.999999999879999546, -2.250000000000000000, -135.0552959530000123 ) ) ;
#13695 = ORIENTED_EDGE ( 'NONE', *, *, #4090, .T. ) ;
#13696 = CARTESIAN_POINT ( 'NONE',  ( -16.46253290489252663, 36.15891006124687834, -139.5597335927451752 ) ) ;
#13697 = CARTESIAN_POINT ( 'NONE',  ( 31.50000000000000000, 32.96379895120000469, -136.5552959530000123 ) ) ;
#13698 = DIRECTION ( 'NONE',  ( 1.000000000000000000, 0.000000000000000000, -2.854859206178974232E-14 ) ) ;
#13699 = CARTESIAN_POINT ( 'NONE',  ( -4.584402860569999127, 37.05223431090000474, -140.2914745300000163 ) ) ;
#13700 = DIRECTION ( 'NONE',  ( 2.257144641399999941E-12, -8.049635416090000264E-35, 1.000000000000000000 ) ) ;
#13701 = VECTOR ( 'NONE', #10811, 1000.000000000000000 ) ;
#13702 = VECTOR ( 'NONE', #13638, 1000.000000000000000 ) ;
#13703 = ORIENTED_EDGE ( 'NONE', *, *, #1239, .T. ) ;
#13704 = CARTESIAN_POINT ( 'NONE',  ( -9.958372260283605115, 33.77808441015003638, -141.9208523075240009 ) ) ;
#13705 = FACE_OUTER_BOUND ( 'NONE', #10640, .T. ) ;
#13706 = CARTESIAN_POINT ( 'NONE',  ( 4.301424340778726929, -1.999932770097490042, -150.0552959529999839 ) ) ;
#13707 = EDGE_CURVE ( 'NONE', #19082, #18664, #10732, .T. ) ;
#13708 = ORIENTED_EDGE ( 'NONE', *, *, #22327, .T. ) ;
#13709 = CARTESIAN_POINT ( 'NONE',  ( 2.500000000130000011, 20.50000000000000000, -150.5552959529999839 ) ) ;
#13710 = LINE ( 'NONE', #12268, #20507 ) ;
#13711 = CARTESIAN_POINT ( 'NONE',  ( -5.500000000000000000, 44.50000000000000000, -151.0552959529999839 ) ) ;
#13712 = VERTEX_POINT ( 'NONE', #13463 ) ;
#13713 = CARTESIAN_POINT ( 'NONE',  ( -24.30767937719999949, 40.97374044589999897, -144.4830919949999952 ) ) ;
#13714 = PRODUCT_RELATED_PRODUCT_CATEGORY ( 'part', '', ( #179 ) ) ;
#13715 = DIRECTION ( 'NONE',  ( 2.257171095940000041E-12, 1.003664318210000046E-28, 1.000000000000000000 ) ) ;
#13716 = EDGE_CURVE ( 'NONE', #2388, #22098, #11663, .T. ) ;
#13717 = CARTESIAN_POINT ( 'NONE',  ( -15.24898703719208193, 36.96741147810104877, -148.5896301378323301 ) ) ;
#13718 = DIRECTION ( 'NONE',  ( -2.023844055306273103E-15, -1.000000000000000000, 0.000000000000000000 ) ) ;
#13719 = CARTESIAN_POINT ( 'NONE',  ( -9.776657394585679839, 32.72643639172331120, -146.2409476793991416 ) ) ;
#13720 = VECTOR ( 'NONE', #15743, 1000.000000000000000 ) ;
#13721 = CYLINDRICAL_SURFACE ( 'NONE', #11587, 1.000000000000000888 ) ;
#13722 = CIRCLE ( 'NONE', #14478, 2.000000000000000000 ) ;
#13723 = CARTESIAN_POINT ( 'NONE',  ( 7.053444247323598759, -32.99994780906266811, -150.0552959530000123 ) ) ;
#13724 = ORIENTED_EDGE ( 'NONE', *, *, #3592, .F. ) ;
#13725 = DIRECTION ( 'NONE',  ( 0.000000000000000000, 0.000000000000000000, -1.000000000000000000 ) ) ;
#13726 =( NAMED_UNIT ( * ) SI_UNIT ( $, .STERADIAN. ) SOLID_ANGLE_UNIT ( ) );
#13727 = EDGE_CURVE ( 'NONE', #14370, #1248, #8568, .T. ) ;
#13728 = ORIENTED_EDGE ( 'NONE', *, *, #5491, .F. ) ;
#13729 = PRODUCT_DEFINITION_SHAPE ( 'NONE', 'NONE',  #23545 ) ;
#13730 = CARTESIAN_POINT ( 'NONE',  ( -6.227860603739999945, 35.34754625490000279, -147.7419925389999946 ) ) ;
#13731 = CARTESIAN_POINT ( 'NONE',  ( -28.90798551740000022, 37.01360947639999921, -139.5686590450000040 ) ) ;
#13732 = CARTESIAN_POINT ( 'NONE',  ( -12.50000000000000000, 25.50000000000000000, -136.5552959530000123 ) ) ;
#13733 =( BOUNDED_SURFACE ( )  B_SPLINE_SURFACE ( 5, 5, ( 
 ( #20849, #10117, #22398, #21091, #13462, #4318 ),
 ( #22743, #17033, #19061, #11907, #13349, #20728 ),
 ( #6562, #12025, #20978, #10239, #4543, #17510 ),
 ( #9998, #1233, #11546, #986, #6098, #8217 ),
 ( #18823, #19175, #2535, #6444, #8101, #9757 ),
 ( #2883, #7984, #15262, #22519, #4423, #11662 ),
 ( #2652, #9882, #17155, #875, #6321, #15374 ),
 ( #13575, #15485, #13704, #4667, #17391, #18187 ),
 ( #23426, #5570, #12939, #14726, #19746, #18311 ),
 ( #2026, #2130, #5460, #1905, #12705, #20217 ),
 ( #15727, #10789, #5684, #16515, #9247, #221 ),
 ( #3441, #11147, #6674, #14382, #17959, #18420 ) ),
 .UNSPECIFIED., .F., .F., .F. ) 
 B_SPLINE_SURFACE_WITH_KNOTS ( ( 6, 3, 3, 6 ),
 ( 6, 6 ),
 ( 0.000000000000000000, 4.570086947620000117, 8.869210483019999813, 12.91901055009999943 ),
 ( 0.000000000000000000, 1.570796326852889946 ),
 .UNSPECIFIED. ) 
 GEOMETRIC_REPRESENTATION_ITEM ( )  RATIONAL_B_SPLINE_SURFACE ( (
 ( 1.000000000000000000, 0.5999999999852579924, 0.3999999999852579813, 0.2999999999889434998, 0.2499999999926290073, 0.2500000000000000000),
 ( 1.000000000000000000, 0.5999999999852579924, 0.3999999999852579813, 0.2999999999889434998, 0.2499999999926290073, 0.2500000000000000000),
 ( 1.000000000000000000, 0.5999999999852579924, 0.3999999999852579813, 0.2999999999889434998, 0.2499999999926290073, 0.2500000000000000000),
 ( 1.000000000000000000, 0.5999999999852579924, 0.3999999999852579813, 0.2999999999889434998, 0.2499999999926290073, 0.2500000000000000000),
 ( 1.000000000000000000, 0.5999999999852579924, 0.3999999999852579813, 0.2999999999889434998, 0.2499999999926290073, 0.2500000000000000000),
 ( 1.000000000000000000, 0.5999999999852579924, 0.3999999999852579813, 0.2999999999889434998, 0.2499999999926290073, 0.2500000000000000000),
 ( 1.000000000000000000, 0.5999999999852579924, 0.3999999999852579813, 0.2999999999889434998, 0.2499999999926290073, 0.2500000000000000000),
 ( 1.000000000000000000, 0.5999999999852579924, 0.3999999999852579813, 0.2999999999889434998, 0.2499999999926290073, 0.2500000000000000000),
 ( 1.000000000000000000, 0.5999999999852579924, 0.3999999999852579813, 0.2999999999889434998, 0.2499999999926290073, 0.2500000000000000000),
 ( 1.000000000000000000, 0.5999999999852579924, 0.3999999999852579813, 0.2999999999889434998, 0.2499999999926290073, 0.2500000000000000000),
 ( 1.000000000000000000, 0.5999999999852579924, 0.3999999999852579813, 0.2999999999889434998, 0.2499999999926290073, 0.2500000000000000000),
 ( 1.000000000000000000, 0.5999999999852579924, 0.3999999999852579813, 0.2999999999889434998, 0.2499999999926290073, 0.2500000000000000000) ) ) 
 REPRESENTATION_ITEM ( '' )  SURFACE ( )  );
#13734 = EDGE_LOOP ( 'NONE', ( #1682, #10842, #189, #3971, #12462, #3501 ) ) ;
#13735 = DIRECTION ( 'NONE',  ( 2.257144641397284947E-12, 2.714760815920564689E-24, 1.000000000000000000 ) ) ;
#13736 = LINE ( 'NONE', #18130, #2672 ) ;
#13737 = VECTOR ( 'NONE', #43, 1000.000000000000000 ) ;
#13738 = EDGE_CURVE ( 'NONE', #13428, #10483, #20255, .T. ) ;
#13739 = ORIENTED_EDGE ( 'NONE', *, *, #936, .T. ) ;
#13740 = VECTOR ( 'NONE', #2273, 1000.000000000000000 ) ;
#13741 = CARTESIAN_POINT ( 'NONE',  ( -21.78779062148921497, 39.33326857531331910, -147.2076583194208013 ) ) ;
#13742 = CARTESIAN_POINT ( 'NONE',  ( -18.75277607359999976, 37.97046254950000588, -148.4181951110000171 ) ) ;
#13743 = CARTESIAN_POINT ( 'NONE',  ( -14.60730091830128252, -40.00000000000000711, -150.0552959530000123 ) ) ;
#13744 = CARTESIAN_POINT ( 'NONE',  ( 7.000013276238538751, 37.20094785582138286, -146.5552931460549075 ) ) ;
#13745 = DIRECTION ( 'NONE',  ( 0.000000000000000000, -1.000000000000000000, 0.000000000000000000 ) ) ;
#13746 = EDGE_CURVE ( 'NONE', #10483, #14227, #15375, .T. ) ;
#13747 = CARTESIAN_POINT ( 'NONE',  ( -25.18773796597552916, 33.56545492220686100, -143.6970596393699964 ) ) ;
#13748 = DIRECTION ( 'NONE',  ( -1.000000000000000000, 5.094701932209999624E-24, 2.257144641399999941E-12 ) ) ;
#13749 = ADVANCED_FACE ( 'NONE', ( #11312, #22282, #15137, #7754, #20623, #5973, #13225, #18721, #2429, #9646, #6099, #5020 ), #19540, .T. ) ;
#13750 = CARTESIAN_POINT ( 'NONE',  ( -12.13467478867948124, 40.69160539494399842, -144.5327625260007665 ) ) ;
#13751 = ORIENTED_EDGE ( 'NONE', *, *, #7911, .F. ) ;
#13752 = DIRECTION ( 'NONE',  ( 0.000000000000000000, -1.000000000000000000, 8.159623473500000156E-13 ) ) ;
#13753 = VECTOR ( 'NONE', #9371, 1000.000000000000000 ) ;
#13754 = AXIS2_PLACEMENT_3D ( 'NONE', #22654, #6349, #13603 ) ;
#13755 = UNCERTAINTY_MEASURE_WITH_UNIT (LENGTH_MEASURE( 1.000000000000000082E-05 ), #17237, 'distance_accuracy_value', 'NONE');
#13756 = AXIS2_PLACEMENT_3D ( 'NONE', #6789, #6557, #19171 ) ;
#13757 = ORIENTED_EDGE ( 'NONE', *, *, #16800, .T. ) ;
#13758 =( NAMED_UNIT ( * ) PLANE_ANGLE_UNIT ( ) SI_UNIT ( $, .RADIAN. ) );
#13759 = ADVANCED_FACE ( 'NONE', ( #10466 ), #22744, .T. ) ;
#13760 = VERTEX_POINT ( 'NONE', #10000 ) ;
#13761 = CARTESIAN_POINT ( 'NONE',  ( 10.00000000010000001, 37.00000000000000000, -142.5552959529999839 ) ) ;
#13762 = ADVANCED_FACE ( 'NONE', ( #8338 ), #3007, .T. ) ;
#13763 = ORIENTED_EDGE ( 'NONE', *, *, #16266, .T. ) ;
#13764 = CARTESIAN_POINT ( 'NONE',  ( 1.133692148650000009, -51.00000000000000000, -136.0552959530000123 ) ) ;
#13765 = VERTEX_POINT ( 'NONE', #12264 ) ;
#13766 = EDGE_CURVE ( 'NONE', #18172, #10602, #14061, .T. ) ;
#13767 = EDGE_LOOP ( 'NONE', ( #23497, #10542, #15755, #17709 ) ) ;
#13768 = CARTESIAN_POINT ( 'NONE',  ( -31.00000000000000000, -36.00000000000000000, -149.5552959529999839 ) ) ;
#13769 = ADVANCED_FACE ( 'NONE', ( #10240 ), #15486, .T. ) ;
#13770 = CARTESIAN_POINT ( 'NONE',  ( -19.08835673601252836, 35.67218568070619966, -147.3285224709407260 ) ) ;
#13771 = CARTESIAN_POINT ( 'NONE',  ( -10.86836323999999898, 38.91206754959999614, -139.9811931129999891 ) ) ;
#13772 = DIRECTION ( 'NONE',  ( 0.000000000000000000, 1.000000000000000000, 0.000000000000000000 ) ) ;
#13773 = DIRECTION ( 'NONE',  ( 8.952838470580000762E-12, -9.094947017729999296E-13, 1.000000000000000000 ) ) ;
#13774 = DIRECTION ( 'NONE',  ( -1.000000000000000000, 0.000000000000000000, 2.259525899719999991E-12 ) ) ;
#13775 = ORIENTED_EDGE ( 'NONE', *, *, #14469, .T. ) ;
#13776 = CARTESIAN_POINT ( 'NONE',  ( -27.80359210600000353, 32.89696731220000459, -146.3345487529999787 ) ) ;
#13777 =( GEOMETRIC_REPRESENTATION_CONTEXT ( 3 ) GLOBAL_UNCERTAINTY_ASSIGNED_CONTEXT ( ( #17788 ) ) GLOBAL_UNIT_ASSIGNED_CONTEXT ( ( #10018, #774, #15390 ) ) REPRESENTATION_CONTEXT ( 'NONE', 'WORKASPACE' ) );
#13778 = VECTOR ( 'NONE', #2849, 1000.000000000000000 ) ;
#13779 = LINE ( 'NONE', #19237, #4911 ) ;
#13780 = FACE_OUTER_BOUND ( 'NONE', #10869, .T. ) ;
#13781 = VERTEX_POINT ( 'NONE', #20979 ) ;
#13782 = DIRECTION ( 'NONE',  ( -0.7633862853691523176, 0.6459422414661291079, 0.000000000000000000 ) ) ;
#13783 = DIRECTION ( 'NONE',  ( 2.257144641399999941E-12, -4.009147065136860232E-51, 1.000000000000000000 ) ) ;
#13784 = ORIENTED_EDGE ( 'NONE', *, *, #15631, .F. ) ;
#13785 = DIRECTION ( 'NONE',  ( -2.257115129720000004E-12, 0.000000000000000000, -1.000000000000000000 ) ) ;
#13786 = LINE ( 'NONE', #4621, #2890 ) ;
#13787 = ORIENTED_EDGE ( 'NONE', *, *, #16736, .T. ) ;
#13788 = DIRECTION ( 'NONE',  ( -3.994014902717275590E-29, 1.000000000000000000, -4.148443855747225317E-27 ) ) ;
#13789 = DIRECTION ( 'NONE',  ( 2.257144641399999941E-12, -8.049635444003269754E-35, 1.000000000000000000 ) ) ;
#13790 = ORIENTED_EDGE ( 'NONE', *, *, #20162, .T. ) ;
#13791 = CARTESIAN_POINT ( 'NONE',  ( -14.24884431174197452, 36.97292245484901230, -139.4994906131649088 ) ) ;
#13792 = ADVANCED_FACE ( 'NONE', ( #6445 ), #15613, .F. ) ;
#13793 = CARTESIAN_POINT ( 'NONE',  ( -25.54709891099935959, 36.13246793449779659, -139.7173810944768206 ) ) ;
#13794 = MECHANICAL_DESIGN_GEOMETRIC_PRESENTATION_REPRESENTATION (  '', ( #13037 ), #8083 ) ;
#13795 = ORIENTED_EDGE ( 'NONE', *, *, #7673, .T. ) ;
#13796 =( NAMED_UNIT ( * ) SI_UNIT ( $, .STERADIAN. ) SOLID_ANGLE_UNIT ( ) );
#13797 = LINE ( 'NONE', #21498, #2056 ) ;
#13798 = EDGE_LOOP ( 'NONE', ( #10786, #3063, #21761, #39 ) ) ;
#13799 = CARTESIAN_POINT ( 'NONE',  ( -11.58731752079999922, 38.53682247849999953, -140.5940415739999878 ) ) ;
#13800 = DIRECTION ( 'NONE',  ( 0.000000000000000000, 1.000000000000000000, 0.000000000000000000 ) ) ;
#13801 = ORIENTED_EDGE ( 'NONE', *, *, #4226, .F. ) ;
#13802 = DIRECTION ( 'NONE',  ( 2.257144641399999941E-12, 0.000000000000000000, -1.000000000000000000 ) ) ;
#13803 = ORIENTED_EDGE ( 'NONE', *, *, #2136, .T. ) ;
#13804 = DIRECTION ( 'NONE',  ( 1.701177084980000217E-20, 4.426606872460000157E-37, 1.000000000000000000 ) ) ;
#13805 = DIRECTION ( 'NONE',  ( 0.000000000000000000, -2.252420472359999842E-12, -1.000000000000000000 ) ) ;
#13806 = ORIENTED_EDGE ( 'NONE', *, *, #768, .F. ) ;
#13807 = PRESENTATION_LAYER_ASSIGNMENT (  '', '', ( #2425 ) ) ;
#13808 = ORIENTED_EDGE ( 'NONE', *, *, #2589, .F. ) ;
#13809 = CARTESIAN_POINT ( 'NONE',  ( -3.499999999959999997, 44.50000000000000000, -136.0552959530000123 ) ) ;
#13810 = LINE ( 'NONE', #21073, #15775 ) ;
#13811 = CARTESIAN_POINT ( 'NONE',  ( -14.21887350778302128, 37.71951061619743939, -140.5431489171175770 ) ) ;
#13812 = DIRECTION ( 'NONE',  ( 5.094701932209999624E-24, 1.000000000000000000, -1.149947916579999802E-35 ) ) ;
#13813 = ORIENTED_EDGE ( 'NONE', *, *, #2127, .T. ) ;
#13814 = CARTESIAN_POINT ( 'NONE',  ( 32.50000000000000000, 20.96379895120000114, -136.5552959530000123 ) ) ;
#13815 = DIRECTION ( 'NONE',  ( -0.1309625047069831461, -0.9913873220698726785, 3.575326271489538320E-13 ) ) ;
#13816 = CARTESIAN_POINT ( 'NONE',  ( 21.10099947280545507, -18.65635984007526105, -150.0552959529999839 ) ) ;
#13817 = CARTESIAN_POINT ( 'NONE',  ( -16.46189020600415631, -42.60961311590466494, -150.0552959530000408 ) ) ;
#13818 = DIRECTION ( 'NONE',  ( 0.000000000000000000, 1.000000000000000000, 0.000000000000000000 ) ) ;
#13819 = ADVANCED_FACE ( 'NONE', ( #13705 ), #21329, .T. ) ;
#13820 = DIRECTION ( 'NONE',  ( 1.000000000000000000, 0.000000000000000000, -2.262079412673756451E-12 ) ) ;
#13821 = ORIENTED_EDGE ( 'NONE', *, *, #22193, .F. ) ;
#13822 = CARTESIAN_POINT ( 'NONE',  ( -16.72278394149610037, 36.31586521337584372, -140.5063707124861878 ) ) ;
#13823 = DIRECTION ( 'NONE',  ( 1.000000000000000000, 2.602084704489999637E-17, -1.701177084980000217E-20 ) ) ;
#13824 = CARTESIAN_POINT ( 'NONE',  ( 6.500000000000000000, 20.50000000000000000, -151.0552959529999839 ) ) ;
#13825 = CARTESIAN_POINT ( 'NONE',  ( -5.271986118780927377, 36.97016010513713979, -139.4665544805324657 ) ) ;
#13826 = FACE_OUTER_BOUND ( 'NONE', #5860, .T. ) ;
#13827 = ORIENTED_EDGE ( 'NONE', *, *, #19537, .T. ) ;
#13828 = LINE ( 'NONE', #6214, #16721 ) ;
#13829 = DIRECTION ( 'NONE',  ( 0.9999976651796518290, -0.002160933882609249439, -8.955304954746877373E-12 ) ) ;
#13830 = CARTESIAN_POINT ( 'NONE',  ( 6.000000000000000000, -3.500000000000000000, -150.0552959529999839 ) ) ;
#13831 = ORIENTED_EDGE ( 'NONE', *, *, #7235, .F. ) ;
#13832 =( NAMED_UNIT ( * ) SI_UNIT ( $, .STERADIAN. ) SOLID_ANGLE_UNIT ( ) );
#13833 = CARTESIAN_POINT ( 'NONE',  ( -28.88704352681202536, 32.48182513811993744, -143.5726213976734584 ) ) ;
#13834 = LINE ( 'NONE', #21097, #8313 ) ;
#13835 = ORIENTED_EDGE ( 'NONE', *, *, #15497, .T. ) ;
#13836 = CARTESIAN_POINT ( 'NONE',  ( -23.48449349015638887, 36.94479390616790937, -140.4349842069408112 ) ) ;
#13837 = CARTESIAN_POINT ( 'NONE',  ( -35.73252798949999942, 37.00000000000000000, -138.5552959529999839 ) ) ;
#13838 = CARTESIAN_POINT ( 'NONE',  ( 3.249999999879999990, -4.000000000000000000, -135.0552959530000123 ) ) ;
#13839 = CARTESIAN_POINT ( 'NONE',  ( 6.750000000000000000, -36.00000000000000000, -151.0552959529999839 ) ) ;
#13840 = CARTESIAN_POINT ( 'NONE',  ( -5.064279449469999861, 40.47653686799999662, -142.0698957560000224 ) ) ;
#13841 = CARTESIAN_POINT ( 'NONE',  ( -0.009371101363106103949, 24.25767361204312067, -150.0552959529999839 ) ) ;
#13842 = CARTESIAN_POINT ( 'NONE',  ( 3.736991614091279335, -36.11279581097431901, -150.0552959529999839 ) ) ;
#13843 = EDGE_CURVE ( 'NONE', #384, #21164, #5127, .T. ) ;
#13844 = AXIS2_PLACEMENT_3D ( 'NONE', #6350, #18965, #545 ) ;
#13845 = ORIENTED_EDGE ( 'NONE', *, *, #15215, .T. ) ;
#13846 = ADVANCED_FACE ( 'NONE', ( #10357 ), #6916, .F. ) ;
#13847 = SURFACE_STYLE_USAGE ( .BOTH. , #21228 ) ;
#13848 = ORIENTED_EDGE ( 'NONE', *, *, #3842, .F. ) ;
#13849 = CARTESIAN_POINT ( 'NONE',  ( -8.168564777796522236, 34.74583461989782052, -141.1491392514008680 ) ) ;
#13850 = CARTESIAN_POINT ( 'NONE',  ( -26.50527565049999978, 41.51083911109999747, -144.5405030839999938 ) ) ;
#13851 = LINE ( 'NONE', #13732, #11540 ) ;
#13852 = ORIENTED_EDGE ( 'NONE', *, *, #1543, .T. ) ;
#13853 = CARTESIAN_POINT ( 'NONE',  ( 2.508811538200000246, -14.35090895149999923, -144.5552959529999839 ) ) ;
#13854 = DIRECTION ( 'NONE',  ( 0.7633862853691523176, 0.6459422414661291079, 0.000000000000000000 ) ) ;
#13855 = ORIENTED_EDGE ( 'NONE', *, *, #3740, .F. ) ;
#13856 = FACE_OUTER_BOUND ( 'NONE', #6456, .T. ) ;
#13857 = CARTESIAN_POINT ( 'NONE',  ( -18.04274282227677872, 40.84322841768359780, -141.6905766441785488 ) ) ;
#13858 = DIRECTION ( 'NONE',  ( 2.602084704489999637E-17, -1.000000000000000000, -4.426606872070000353E-37 ) ) ;
#13859 = FACE_BOUND ( 'NONE', #8178, .T. ) ;
#13860 = EDGE_CURVE ( 'NONE', #17719, #903, #879, .T. ) ;
#13861 = CARTESIAN_POINT ( 'NONE',  ( -32.50000000000000000, -43.00000000000000000, -137.0552959530000123 ) ) ;
#13862 = CARTESIAN_POINT ( 'NONE',  ( -25.44349950041027952, 35.21826511839348228, -139.9516901547978023 ) ) ;
#13863 = FACE_OUTER_BOUND ( 'NONE', #17601, .T. ) ;
#13864 = CARTESIAN_POINT ( 'NONE',  ( -3.238200612160851755, 42.50000000000000711, -136.0552959530006092 ) ) ;
#13865 = EDGE_LOOP ( 'NONE', ( #4514, #16989, #17802, #15806 ) ) ;
#13866 = LINE ( 'NONE', #8022, #5254 ) ;
#13867 = EDGE_CURVE ( 'NONE', #15451, #21143, #22876, .T. ) ;
#13868 = ORIENTED_EDGE ( 'NONE', *, *, #10525, .F. ) ;
#13869 = ORIENTED_EDGE ( 'NONE', *, *, #13262, .F. ) ;
#13870 = ORIENTED_EDGE ( 'NONE', *, *, #8128, .T. ) ;
#13871 = VECTOR ( 'NONE', #18455, 1000.000000000000000 ) ;
#13872 = DIRECTION ( 'NONE',  ( -2.602084747549999882E-17, 1.000000000000000000, 5.873289694040000105E-29 ) ) ;
#13873 = CARTESIAN_POINT ( 'NONE',  ( -31.50000000000000000, -43.00000000000000000, -137.0552959530000123 ) ) ;
#13874 = VERTEX_POINT ( 'NONE', #12026 ) ;
#13875 = VERTEX_POINT ( 'NONE', #19297 ) ;
#13876 = DIRECTION ( 'NONE',  ( 0.000000000000000000, -1.000000000000000000, 0.000000000000000000 ) ) ;
#13877 = EDGE_CURVE ( 'NONE', #15726, #10697, #17511, .T. ) ;
#13878 = CARTESIAN_POINT ( 'NONE',  ( -8.712023184210000437, 38.57885015669999973, -140.3122811009999964 ) ) ;
#13879 = FACE_OUTER_BOUND ( 'NONE', #2746, .T. ) ;
#13880 = CARTESIAN_POINT ( 'NONE',  ( -21.35824191589811605, -3.250000000000000000, -146.3157682190075093 ) ) ;
#13881 = CARTESIAN_POINT ( 'NONE',  ( -8.565647946495506204, 36.93510680650897626, -139.7232782068719530 ) ) ;
#13882 = CARTESIAN_POINT ( 'NONE',  ( 8.900000000049999471, 34.53220746410000430, -149.1552959530000066 ) ) ;
#13883 = ORIENTED_EDGE ( 'NONE', *, *, #22820, .F. ) ;
#13884 = FACE_OUTER_BOUND ( 'NONE', #12322, .T. ) ;
#13885 = EDGE_CURVE ( 'NONE', #11596, #4470, #6675, .T. ) ;
#13886 = DIRECTION ( 'NONE',  ( -1.000000000000000000, 1.458293570536846221E-24, 2.257144641401985094E-12 ) ) ;
#13887 = ADVANCED_FACE ( 'NONE', ( #12146 ), #17632, .T. ) ;
#13888 = VECTOR ( 'NONE', #18955, 1000.000000000000227 ) ;
#13889 = LINE ( 'NONE', #17586, #19754 ) ;
#13890 = CIRCLE ( 'NONE', #13136, 4.000000000000003553 ) ;
#13891 = ORIENTED_EDGE ( 'NONE', *, *, #13158, .T. ) ;
#13892 = EDGE_CURVE ( 'NONE', #17215, #8780, #13019, .T. ) ;
#13893 = EDGE_CURVE ( 'NONE', #7320, #8811, #21918, .T. ) ;
#13894 = DIRECTION ( 'NONE',  ( -1.000000000000000000, 0.000000000000000000, 2.257144641399999941E-12 ) ) ;
#13895 = ORIENTED_EDGE ( 'NONE', *, *, #14733, .T. ) ;
#13896 = DIRECTION ( 'NONE',  ( 1.000000000000000000, 0.000000000000000000, -2.267228047249999995E-12 ) ) ;
#13897 = ORIENTED_EDGE ( 'NONE', *, *, #5038, .T. ) ;
#13898 = CARTESIAN_POINT ( 'NONE',  ( 0.000000000000000000, 21.50000000000000000, -150.0552959529999839 ) ) ;
#13899 = CARTESIAN_POINT ( 'NONE',  ( -18.85469010170000459, 37.03971195569999963, -148.4264296979999926 ) ) ;
#13900 = ORIENTED_EDGE ( 'NONE', *, *, #18983, .T. ) ;
#13901 = DIRECTION ( 'NONE',  ( 0.000000000000000000, -0.4794255386042033384, -0.8775825618903726477 ) ) ;
#13902 = CARTESIAN_POINT ( 'NONE',  ( -26.31398817765400011, 34.53172810853797614, -140.8131697956154653 ) ) ;
#13903 = ORIENTED_EDGE ( 'NONE', *, *, #20716, .T. ) ;
#13904 = EDGE_LOOP ( 'NONE', ( #3655, #22208, #22256, #1812, #15823 ) ) ;
#13905 = CARTESIAN_POINT ( 'NONE',  ( -12.13467478879999994, 40.69160539509999808, -144.5327625259999706 ) ) ;
#13906 = VECTOR ( 'NONE', #3689, 1000.000000000000000 ) ;
#13907 = CARTESIAN_POINT ( 'NONE',  ( 6.000000000160000013, 41.50000000000000000, -140.5552959529999839 ) ) ;
#13908 = VERTEX_POINT ( 'NONE', #9031 ) ;
#13909 = AXIS2_PLACEMENT_3D ( 'NONE', #17997, #5381, #20138 ) ;
#13910 = DIRECTION ( 'NONE',  ( 0.000000000000000000, 1.000000000000000000, 0.000000000000000000 ) ) ;
#13911 = EDGE_CURVE ( 'NONE', #1861, #10881, #11362, .T. ) ;
#13912 = PLANE ( 'NONE',  #20491 ) ;
#13913 = DIRECTION ( 'NONE',  ( 0.000000000000000000, 0.000000000000000000, -1.000000000000000000 ) ) ;
#13914 = EDGE_CURVE ( 'NONE', #12665, #22329, #8808, .T. ) ;
#13915 = EDGE_CURVE ( 'NONE', #2213, #12155, #28, .T. ) ;
#13916 = ORIENTED_EDGE ( 'NONE', *, *, #16490, .F. ) ;
#13917 = CARTESIAN_POINT ( 'NONE',  ( 4.107300918301270976, -0.5000000000000004441, -150.0552959529999839 ) ) ;
#13918 = LINE ( 'NONE', #22855, #7415 ) ;
#13919 = CARTESIAN_POINT ( 'NONE',  ( -14.83261257093395180, 37.83839852817070692, -148.3884378576142922 ) ) ;
#13920 = CARTESIAN_POINT ( 'NONE',  ( -34.50000000000000000, 48.00000000000000000, -148.5552959529999839 ) ) ;
#13921 = AXIS2_PLACEMENT_3D ( 'NONE', #3622, #7184, #12767 ) ;
#13922 = ORIENTED_EDGE ( 'NONE', *, *, #5957, .F. ) ;
#13923 = LINE ( 'NONE', #4880, #16259 ) ;
#13924 = FACE_OUTER_BOUND ( 'NONE', #13541, .T. ) ;
#13925 = CARTESIAN_POINT ( 'NONE',  ( -9.334216945200001447, -17.19633444960000190, -146.5552959529999839 ) ) ;
#13926 = LINE ( 'NONE', #2991, #10613 ) ;
#13927 = CARTESIAN_POINT ( 'NONE',  ( -20.60824191589999899, -32.00000000000000000, -146.2257682199999920 ) ) ;
#13928 = CARTESIAN_POINT ( 'NONE',  ( 22.42370904790000097, -21.41421288319999761, -142.5552959529999839 ) ) ;
#13929 = ORIENTED_EDGE ( 'NONE', *, *, #18117, .F. ) ;
#13930 = CARTESIAN_POINT ( 'NONE',  ( 15.50000000000000000, 39.50000000000000000, -150.5552959529999839 ) ) ;
#13931 = CARTESIAN_POINT ( 'NONE',  ( -6.370493725010000219, -17.65251768590000125, -144.5552959529999839 ) ) ;
#13932 = CARTESIAN_POINT ( 'NONE',  ( -31.00000000000000000, -50.50000000000000000, -149.5552959529999839 ) ) ;
#13933 = CARTESIAN_POINT ( 'NONE',  ( -34.50000000000000000, 28.00000000000000000, -146.5552959529999839 ) ) ;
#13934 = PLANE ( 'NONE',  #8131 ) ;
#13935 = ORIENTED_EDGE ( 'NONE', *, *, #16426, .F. ) ;
#13936 = FACE_OUTER_BOUND ( 'NONE', #13148, .T. ) ;
#13937 = CARTESIAN_POINT ( 'NONE',  ( -2.499999999920000437, 40.00000000000000000, -136.5552959530000123 ) ) ;
#13938 = VECTOR ( 'NONE', #9360, 1000.000000000000000 ) ;
#13939 = CARTESIAN_POINT ( 'NONE',  ( -32.50000000000000000, 28.00000000000000000, -141.5552959529999839 ) ) ;
#13940 = ORIENTED_EDGE ( 'NONE', *, *, #20145, .T. ) ;
#13941 = ADVANCED_FACE ( 'NONE', ( #19776 ), #20126, .F. ) ;
#13942 = CARTESIAN_POINT ( 'NONE',  ( -28.50747929780000334, 33.37084171139999711, -143.6371486329999811 ) ) ;
#13943 = CARTESIAN_POINT ( 'NONE',  ( 29.68320006080000084, -24.50000000000000000, -150.0552959529999839 ) ) ;
#13944 = EDGE_LOOP ( 'NONE', ( #4048, #5904, #16921, #20580, #137, #17749, #16963, #6043 ) ) ;
#13945 = CARTESIAN_POINT ( 'NONE',  ( -23.55797472143900251, 40.74841938861488444, -146.3388075608100110 ) ) ;
#13946 = LINE ( 'NONE', #6927, #20759 ) ;
#13947 = CARTESIAN_POINT ( 'NONE',  ( -32.50000000000000000, 48.00000000000000000, -150.5552959529999839 ) ) ;
#13948 = PLANE ( 'NONE',  #10219 ) ;
#13949 = ORIENTED_EDGE ( 'NONE', *, *, #21861, .T. ) ;
#13950 = CARTESIAN_POINT ( 'NONE',  ( -9.544641620896076262, 34.08278316542619990, -147.7344509276062752 ) ) ;
#13951 = CARTESIAN_POINT ( 'NONE',  ( 6.007013984441634591, 28.00000000000000000, -150.0552959529999839 ) ) ;
#13952 = AXIS2_PLACEMENT_3D ( 'NONE', #666, #22205, #7556 ) ;
#13953 = DIRECTION ( 'NONE',  ( 0.000000000000000000, 1.000000000000000000, -2.273736754430000208E-12 ) ) ;
#13954 = PLANE ( 'NONE',  #19810 ) ;
#13955 = ORIENTED_EDGE ( 'NONE', *, *, #15313, .T. ) ;
#13956 = COLOUR_RGB ( '', 0.66274510, 0.83137255, 0.94901961) ;
#13957 = CARTESIAN_POINT ( 'NONE',  ( -20.85361110351559333, 37.81545827817836170, -148.3531455720921031 ) ) ;
#13958 = PRESENTATION_STYLE_ASSIGNMENT (( #23009 ) ) ;
#13959 = AXIS2_PLACEMENT_3D ( 'NONE', #13993, #23284, #21390 ) ;
#13960 = ORIENTED_EDGE ( 'NONE', *, *, #14904, .T. ) ;
#13961 = CARTESIAN_POINT ( 'NONE',  ( -7.284577139200968610, 35.45677114639833150, -140.5143805028650377 ) ) ;
#13962 = DIRECTION ( 'NONE',  ( 1.000000000000000000, 0.000000000000000000, 0.000000000000000000 ) ) ;
#13963 = LINE ( 'NONE', #4692, #5105 ) ;
#13964 = ORIENTED_EDGE ( 'NONE', *, *, #22165, .F. ) ;
#13965 = CARTESIAN_POINT ( 'NONE',  ( -2.499999999859999988, 20.50000000000000000, -146.5552959529999839 ) ) ;
#13966 = DIRECTION ( 'NONE',  ( 1.000000000000000000, 0.000000000000000000, -4.511206223393553012E-12 ) ) ;
#13967 = ORIENTED_EDGE ( 'NONE', *, *, #22617, .F. ) ;
#13968 = DIRECTION ( 'NONE',  ( 1.000000000000000000, 0.000000000000000000, -2.257453483404482811E-12 ) ) ;
#13969 = EDGE_CURVE ( 'NONE', #7704, #10902, #12735, .T. ) ;
#13970 = CARTESIAN_POINT ( 'NONE',  ( -18.31895680040000229, 41.06933176500000116, -146.2870363079999834 ) ) ;
#13971 = AXIS2_PLACEMENT_3D ( 'NONE', #22009, #11863, #17111 ) ;
#13972 = CARTESIAN_POINT ( 'NONE',  ( -25.64792992860000354, 37.04465132570000208, -139.7265440090000084 ) ) ;
#13973 = EDGE_CURVE ( 'NONE', #16462, #13434, #18221, .T. ) ;
#13974 = LINE ( 'NONE', #7069, #17857 ) ;
#13975 = DIRECTION ( 'NONE',  ( -4.511946372079999833E-12, 1.314504061159999897E-13, -1.000000000000000000 ) ) ;
#13976 = DIRECTION ( 'NONE',  ( 1.000000000000000000, 0.000000000000000000, -4.510281037539699253E-12 ) ) ;
#13977 = DIRECTION ( 'NONE',  ( 0.000000000000000000, 1.000000000000000000, -2.273736754430000208E-12 ) ) ;
#13978 = DIRECTION ( 'NONE',  ( -0.000000000000000000, 1.000000000000000000, 0.000000000000000000 ) ) ;
#13979 = VERTEX_POINT ( 'NONE', #14759 ) ;
#13980 = CARTESIAN_POINT ( 'NONE',  ( -2.499999999920000437, 34.00000000000000000, -136.5552959530000123 ) ) ;
#13982 = ORIENTED_EDGE ( 'NONE', *, *, #16214, .F. ) ;
#13981 = VECTOR ( 'NONE', #4305, 1000.000000000000000 ) ;
#13983 =( NAMED_UNIT ( * ) PLANE_ANGLE_UNIT ( ) SI_UNIT ( $, .RADIAN. ) );
#13984 = VECTOR ( 'NONE', #14491, 1000.000000000000114 ) ;
#13985 = EDGE_LOOP ( 'NONE', ( #2465, #4082, #5642, #5929 ) ) ;
#13986 = CARTESIAN_POINT ( 'NONE',  ( 0.8488726857078380261, 25.45511797032530765, -136.0552959530019450 ) ) ;
#13987 = CARTESIAN_POINT ( 'NONE',  ( -27.77884619099882713, 32.57034656671790174, -143.4578452901890273 ) ) ;
#13988 = ORIENTED_EDGE ( 'NONE', *, *, #9522, .F. ) ;
#13989 = ORIENTED_EDGE ( 'NONE', *, *, #21337, .F. ) ;
#13990 = FACE_OUTER_BOUND ( 'NONE', #1803, .T. ) ;
#13991 = CARTESIAN_POINT ( 'NONE',  ( -9.005502668700000157, 40.51905748810000318, -141.9284054809999986 ) ) ;
#13992 = CARTESIAN_POINT ( 'NONE',  ( -11.86981903014650008, 40.35288497626832083, -142.1893091612195974 ) ) ;
#13993 = CARTESIAN_POINT ( 'NONE',  ( 1.000000000160000013, 36.50000000000000000, -140.5552959529999839 ) ) ;
#13994 = CARTESIAN_POINT ( 'NONE',  ( -7.644488704951585945, 35.02206480932151322, -139.6643986246225779 ) ) ;
#13995 = ORIENTED_EDGE ( 'NONE', *, *, #5801, .T. ) ;
#13996 = CARTESIAN_POINT ( 'NONE',  ( -28.59946202389999925, 34.31616424880000693, -140.2812573680000128 ) ) ;
#13997 = EDGE_CURVE ( 'NONE', #21066, #16352, #3825, .T. ) ;
#13998 = VECTOR ( 'NONE', #7730, 1000.000000000000000 ) ;
#13999 = VECTOR ( 'NONE', #20216, 1000.000000000000000 ) ;
#14000 = CARTESIAN_POINT ( 'NONE',  ( 5.699500263607268913, -4.421820079962375694, -136.0552959530027124 ) ) ;
#14001 = VECTOR ( 'NONE', #17623, 1000.000000000000000 ) ;
#14002 = CARTESIAN_POINT ( 'NONE',  ( 16.61718498210000305, -18.75502267109999721, -142.5552959529999839 ) ) ;
#14003 = ORIENTED_EDGE ( 'NONE', *, *, #21981, .F. ) ;
#14004 = PRODUCT_RELATED_PRODUCT_CATEGORY ( 'part', '', ( #4785 ) ) ;
#14005 = AXIS2_PLACEMENT_3D ( 'NONE', #7246, #16516, #12590 ) ;
#14006 = EDGE_CURVE ( 'NONE', #22397, #9000, #9095, .T. ) ;
#14007 = DIRECTION ( 'NONE',  ( 0.000000000000000000, 1.000000000000000000, 0.000000000000000000 ) ) ;
#14008 = ORIENTED_EDGE ( 'NONE', *, *, #22932, .T. ) ;
#14009 = CARTESIAN_POINT ( 'NONE',  ( 7.750000000000000000, -42.23606797749999942, -150.5552959529999839 ) ) ;
#14010 = CARTESIAN_POINT ( 'NONE',  ( 15.85402906740000084, -26.57485422999999969, -145.5552959529999839 ) ) ;
#14011 = ORIENTED_EDGE ( 'NONE', *, *, #11404, .T. ) ;
#14012 = CARTESIAN_POINT ( 'NONE',  ( -19.54668701403429054, 37.05673630841071287, -139.5622637236315029 ) ) ;
#14013 = CARTESIAN_POINT ( 'NONE',  ( 15.59498359470000040, -26.23371093219999750, -147.5552959529999839 ) ) ;
#14014 = VERTEX_POINT ( 'NONE', #16439 ) ;
#14015 = CARTESIAN_POINT ( 'NONE',  ( -32.50000000000000000, 51.50000000000000000, -137.0552959530000123 ) ) ;
#14016 = CARTESIAN_POINT ( 'NONE',  ( -25.78373889329461122, 32.73831349156768056, -141.6589310348909123 ) ) ;
#14017 = ORIENTED_EDGE ( 'NONE', *, *, #20716, .F. ) ;
#14018 =( NAMED_UNIT ( * ) SI_UNIT ( $, .STERADIAN. ) SOLID_ANGLE_UNIT ( ) );
#14019 = VECTOR ( 'NONE', #14326, 1000.000000000000000 ) ;
#14020 = ADVANCED_FACE ( 'NONE', ( #18101 ), #23340, .T. ) ;
#14021 = ORIENTED_EDGE ( 'NONE', *, *, #2432, .T. ) ;
#14022 = DIRECTION ( 'NONE',  ( 0.000000000000000000, 1.000000000000000000, 0.000000000000000000 ) ) ;
#14023 = AXIS2_PLACEMENT_3D ( 'NONE', #19899, #14300, #5251 ) ;
#14024 = DIRECTION ( 'NONE',  ( 2.257171095940000041E-12, 1.003664318210000046E-28, 1.000000000000000000 ) ) ;
#14025 = ORIENTED_EDGE ( 'NONE', *, *, #16069, .T. ) ;
#14026 = CARTESIAN_POINT ( 'NONE',  ( 5.631397321050000571, -17.85059010000000157, -147.5552959529999839 ) ) ;
#14027 = VECTOR ( 'NONE', #15233, 1000.000000000000227 ) ;
#14028 = EDGE_CURVE ( 'NONE', #9252, #22886, #23511, .T. ) ;
#14029 = VECTOR ( 'NONE', #9825, 1000.000000000000000 ) ;
#14030 = CARTESIAN_POINT ( 'NONE',  ( 19.77963439019999825, 51.26338628519999929, -143.0552959529999839 ) ) ;
#14031 = CARTESIAN_POINT ( 'NONE',  ( -24.36912841290000031, 34.40976477760000307, -147.5507798129999912 ) ) ;
#14032 = VERTEX_POINT ( 'NONE', #21563 ) ;
#14033 = CARTESIAN_POINT ( 'NONE',  ( -32.50000000000000000, 16.00000000000000000, -144.0552959529999839 ) ) ;
#14034 = VECTOR ( 'NONE', #4728, 1000.000000000000000 ) ;
#14035 = CARTESIAN_POINT ( 'NONE',  ( -25.86630785139999844, -51.50000000000000000, -134.7421712960000377 ) ) ;
#14036 = EDGE_CURVE ( 'NONE', #8980, #13091, #3470, .T. ) ;
#14037 = AXIS2_PLACEMENT_3D ( 'NONE', #2865, #6424, #6306 ) ;
#14038 = CARTESIAN_POINT ( 'NONE',  ( -13.82941295814141647, 37.74960637515216177, -140.6313136556216250 ) ) ;
#14039 = CARTESIAN_POINT ( 'NONE',  ( -12.50000000000000000, 25.50000000000000000, -150.0552959529999839 ) ) ;
#14040 = ORIENTED_EDGE ( 'NONE', *, *, #17358, .T. ) ;
#14041 = CARTESIAN_POINT ( 'NONE',  ( -15.50000000000000000, 21.50000000000000000, -151.0552959529999839 ) ) ;
#14042 = FACE_BOUND ( 'NONE', #19860, .T. ) ;
#14043 = ADVANCED_FACE ( 'NONE', ( #5373 ), #19893, .F. ) ;
#14044 = AXIS2_PLACEMENT_3D ( 'NONE', #216, #19618, #16509 ) ;
#14045 = CARTESIAN_POINT ( 'NONE',  ( -2.499999999859999988, 41.50000000000000000, -147.5552959529999839 ) ) ;
#14046 = LINE ( 'NONE', #5230, #7886 ) ;
#14047 = CARTESIAN_POINT ( 'NONE',  ( 1.847645635000000119, -15.93876195360000025, -145.5552959529999839 ) ) ;
#14048 = AXIS2_PLACEMENT_3D ( 'NONE', #13420, #8291, #706 ) ;
#14049 = DIRECTION ( 'NONE',  ( 0.000000000000000000, 1.000000000000000000, 0.000000000000000000 ) ) ;
#14050 = VECTOR ( 'NONE', #16082, 1000.000000000000000 ) ;
#14051 = ORIENTED_EDGE ( 'NONE', *, *, #2860, .T. ) ;
#14052 = CARTESIAN_POINT ( 'NONE',  ( -15.82146356845421131, 32.49419957915463186, -143.2970122493755127 ) ) ;
#14053 = EDGE_CURVE ( 'NONE', #8946, #21893, #18448, .T. ) ;
#14054 = DIRECTION ( 'NONE',  ( 0.000000000000000000, 1.000000000000000000, 0.000000000000000000 ) ) ;
#14055 = EDGE_CURVE ( 'NONE', #7796, #5107, #2401, .T. ) ;
#14056 = CARTESIAN_POINT ( 'NONE',  ( 19.68320006079999729, -16.50000000000000000, -148.5552959529999839 ) ) ;
#14057 = CARTESIAN_POINT ( 'NONE',  ( -7.206173031919999694, 35.38491483730000198, -147.9515367340000012 ) ) ;
#14058 = DIRECTION ( 'NONE',  ( -0.9847555042252370550, 0.1739442350240419932, 7.303835699471759765E-15 ) ) ;
#14059 = ADVANCED_FACE ( 'NONE', ( #8076 ), #6071, .T. ) ;
#14060 = VERTEX_POINT ( 'NONE', #4053 ) ;
#14061 = LINE ( 'NONE', #10118, #5438 ) ;
#14062 = CARTESIAN_POINT ( 'NONE',  ( -26.10314130450000292, 34.70878586860000325, -141.0128996759999893 ) ) ;
#14063 = EDGE_LOOP ( 'NONE', ( #13900, #19970, #6751, #11806 ) ) ;
#14064 = VECTOR ( 'NONE', #13029, 1000.000000000000000 ) ;
#14065 = CIRCLE ( 'NONE', #2673, 35.00000000000000000 ) ;
#14066 = VECTOR ( 'NONE', #8506, 1000.000000000000000 ) ;
#14067 = CIRCLE ( 'NONE', #15205, 1.500000000000001332 ) ;
#14068 = CARTESIAN_POINT ( 'NONE',  ( 6.000000000160000013, 36.50000000000000000, -140.0552959529999839 ) ) ;
#14069 = LINE ( 'NONE', #3014, #6420 ) ;
#14070 = ORIENTED_EDGE ( 'NONE', *, *, #13234, .F. ) ;
#14071 = CARTESIAN_POINT ( 'NONE',  ( -23.61748844584506557, 39.23591355021475380, -147.3005354435039749 ) ) ;
#14072 = FACE_OUTER_BOUND ( 'NONE', #13290, .T. ) ;
#14073 = DIRECTION ( 'NONE',  ( 0.000000000000000000, 1.000000000000000000, 0.000000000000000000 ) ) ;
#14074 = CARTESIAN_POINT ( 'NONE',  ( 7.400496094956046989, 38.02196623842161927, -141.7732779964421752 ) ) ;
#14075 = VERTEX_POINT ( 'NONE', #7839 ) ;
#14076 = DIRECTION ( 'NONE',  ( 2.257144641399999941E-12, -4.009147065140000298E-51, 1.000000000000000000 ) ) ;
#14077 = CARTESIAN_POINT ( 'NONE',  ( -0.7601318171633636434, 22.44600007524262963, -150.0552959530000123 ) ) ;
#14078 = CARTESIAN_POINT ( 'NONE',  ( -0.9999999999660000860, 20.50000000000000000, -137.0552959530000123 ) ) ;
#14079 = DIRECTION ( 'NONE',  ( 1.000000000000000000, 2.602084704489999637E-17, -1.701177084980000217E-20 ) ) ;
#14080 = EDGE_LOOP ( 'NONE', ( #21853, #16753, #13988, #20473 ) ) ;
#14081 = AXIS2_PLACEMENT_3D ( 'NONE', #1686, #16186, #23441 ) ;
#14082 = SHAPE_REPRESENTATION ( 'Slotted Screw', ( #5025 ), #10730 ) ;
#14083 = AXIS2_PLACEMENT_3D ( 'NONE', #3762, #3648, #7215 ) ;
#14084 = CARTESIAN_POINT ( 'NONE',  ( -21.63220705389141685, 37.01315499805642162, -148.7192284428339519 ) ) ;
#14085 = EDGE_CURVE ( 'NONE', #320, #18387, #12094, .T. ) ;
#14086 = ORIENTED_EDGE ( 'NONE', *, *, #4224, .T. ) ;
#14087 = CARTESIAN_POINT ( 'NONE',  ( -6.190578628962761343, 36.21727375469096444, -147.6271024187999501 ) ) ;
#14088 = CARTESIAN_POINT ( 'NONE',  ( -21.35824191589999899, -32.00000000000000000, -146.3157682190000060 ) ) ;
#14089 = CARTESIAN_POINT ( 'NONE',  ( 11.20518671956328483, -21.39222690360982426, -148.5552959530000123 ) ) ;
#14090 = ORIENTED_EDGE ( 'NONE', *, *, #8320, .F. ) ;
#14091 = CARTESIAN_POINT ( 'NONE',  ( 16.74346552629999962, -18.31657829129999726, -147.5552959529999839 ) ) ;
#14092 = DIRECTION ( 'NONE',  ( -2.257146850379999957E-12, 0.000000000000000000, -1.000000000000000000 ) ) ;
#14093 = ORIENTED_EDGE ( 'NONE', *, *, #20168, .F. ) ;
#14094 = CARTESIAN_POINT ( 'NONE',  ( 16.74346552629999962, -18.31657829129999726, -147.5552959529999839 ) ) ;
#14095 = DIRECTION ( 'NONE',  ( -2.602084704489999637E-17, 1.000000000000000000, 0.000000000000000000 ) ) ;
#14096 = CARTESIAN_POINT ( 'NONE',  ( -32.50000000000000000, 28.00000000000000000, -146.5552959529999839 ) ) ;
#14097 = CARTESIAN_POINT ( 'NONE',  ( 6.229273316152252882, -46.69892946173250436, -136.0552959530140811 ) ) ;
#14098 = AXIS2_PLACEMENT_3D ( 'NONE', #14311, #21708, #10961 ) ;
#14099 = LINE ( 'NONE', #23261, #10832 ) ;
#14100 = CARTESIAN_POINT ( 'NONE',  ( 23.89222110089999873, -31.59487100459999809, -146.5552959529999839 ) ) ;
#14101 = PRODUCT_CONTEXT ( 'NONE', #17233, 'mechanical' ) ;
#14102 = PLANE ( 'NONE',  #8219 ) ;
#14103 = LINE ( 'NONE', #23381, #19236 ) ;
#14104 = ORIENTED_EDGE ( 'NONE', *, *, #12420, .F. ) ;
#14105 = FACE_OUTER_BOUND ( 'NONE', #20859, .T. ) ;
#14106 = EDGE_CURVE ( 'NONE', #20428, #14361, #3941, .T. ) ;
#14107 = VERTEX_POINT ( 'NONE', #9855 ) ;
#14108 = EDGE_CURVE ( 'NONE', #8290, #6185, #2880, .T. ) ;
#14109 = EDGE_LOOP ( 'NONE', ( #1353, #4714, #7342, #4535 ) ) ;
#14110 = CARTESIAN_POINT ( 'NONE',  ( -15.90674982588249975, 37.04592612750588643, -148.5146100863278491 ) ) ;
#14111 = DIRECTION ( 'NONE',  ( 0.000000000000000000, 1.000000000000000000, 0.000000000000000000 ) ) ;
#14112 = EDGE_CURVE ( 'NONE', #20629, #1, #1494, .T. ) ;
#14113 = ORIENTED_EDGE ( 'NONE', *, *, #3364, .T. ) ;
#14114 = CIRCLE ( 'NONE', #7630, 1.499999999999999556 ) ;
#14115 = CLOSED_SHELL ( 'NONE', ( #20077, #20617, #8255, #14407, #17138, #4429, #2695, #22624, #22034, #18697, #4718, #23195, #18064, #7187, #2482, #20281, #9211, #4254, #16520, #9476, #10810, #7148, #6989, #12567, #20051 ) ) ;
#14116 = COLOUR_RGB ( '', 0.08235294, 0.09019608, 0.10196078) ;
#14117 = B_SPLINE_CURVE_WITH_KNOTS ( 'NONE', 3,
 ( #21405, #22952, #1305, #12333, #10032, #20890, #790, #17424, #20767, #4580, #13493, #21009, #15405, #17308, #1148, #17190, #2570, #4462, #908, #11699, #13744, #2919, #10152, #6486, #18975, #7894, #8380, #4700, #2689, #2457, #15652, #9680, #6359, #9791, #11580, #6244, #22911, #16955, #11822, #11941, #9915, #19096 ),
 .UNSPECIFIED., .F., .F.,
 ( 4, 2, 2, 2, 2, 2, 2, 2, 2, 2, 2, 2, 2, 2, 2, 2, 2, 2, 2, 2, 4 ),
 ( 0.000000000000000000, 0.06250000000000885403, 0.09375000000001450229, 0.1093750000000162370, 0.1250000000000179579, 0.1875000000000174860, 0.2500000000000169864, 0.3125000000000165423, 0.3437500000000161537, 0.3750000000000157652, 0.5000000000000107692, 0.5625000000000061062, 0.5937500000000037748, 0.6250000000000013323, 0.6874999999999966693, 0.7499999999999920064, 0.8124999999999873435, 0.8437499999999847899, 0.8593749999999865663, 0.8749999999999882316, 1.000000000000000000 ),
 .UNSPECIFIED. ) ;
#14118 = VERTEX_POINT ( 'NONE', #11176 ) ;
#14119 = DIRECTION ( 'NONE',  ( 4.430318231639999944E-12, -6.100259101500000139E-13, 1.000000000000000000 ) ) ;
#14120 = CARTESIAN_POINT ( 'NONE',  ( -18.28451977779999993, 36.23520409090000527, -147.6763998119999997 ) ) ;
#14121 = CARTESIAN_POINT ( 'NONE',  ( -12.18289575740000075, 37.87223172089999679, -148.4976681630000144 ) ) ;
#14122 = CARTESIAN_POINT ( 'NONE',  ( -6.363831972638722689, -17.39670249660616363, -147.5552959530002681 ) ) ;
#14123 = CARTESIAN_POINT ( 'NONE',  ( -8.029216439717911769, 32.92480140023701551, -141.8798076613048522 ) ) ;
#14124 = ORIENTED_EDGE ( 'NONE', *, *, #15844, .T. ) ;
#14125 = CARTESIAN_POINT ( 'NONE',  ( 9.736748385090495006, 36.15119022970048235, -141.7037997430031169 ) ) ;
#14126 = EDGE_CURVE ( 'NONE', #4350, #9123, #20703, .T. ) ;
#14127 = CARTESIAN_POINT ( 'NONE',  ( -2.599999999940000084, 37.00000000000000000, -144.0552959529999839 ) ) ;
#14128 = CARTESIAN_POINT ( 'NONE',  ( -32.50000000000000000, 50.00000000000000000, -151.0552959529999839 ) ) ;
#14129 = VECTOR ( 'NONE', #8449, 1000.000000000000000 ) ;
#14130 = ORIENTED_EDGE ( 'NONE', *, *, #19590, .F. ) ;
#14131 = AXIS2_PLACEMENT_3D ( 'NONE', #21587, #5509, #3726 ) ;
#14132 = VECTOR ( 'NONE', #11405, 999.9999999999998863 ) ;
#14133 = LINE ( 'NONE', #17818, #15627 ) ;
#14134 = ORIENTED_EDGE ( 'NONE', *, *, #2979, .T. ) ;
#14135 = DIRECTION ( 'NONE',  ( -1.843274626514380137E-11, 0.000000000000000000, -1.000000000000000000 ) ) ;
#14136 = DIRECTION ( 'NONE',  ( 0.000000000000000000, 1.000000000000000000, 0.000000000000000000 ) ) ;
#14137 = ORIENTED_EDGE ( 'NONE', *, *, #1266, .T. ) ;
#14138 = DIRECTION ( 'NONE',  ( 2.259525899719999991E-12, 0.000000000000000000, 1.000000000000000000 ) ) ;
#14139 = PLANE ( 'NONE',  #12234 ) ;
#14140 = ORIENTED_EDGE ( 'NONE', *, *, #6311, .T. ) ;
#14141 = EDGE_CURVE ( 'NONE', #21927, #17682, #7182, .T. ) ;
#14142 = CARTESIAN_POINT ( 'NONE',  ( -21.23917607311824085, 35.28761490586239802, -147.7082871195992197 ) ) ;
#14143 = CARTESIAN_POINT ( 'NONE',  ( -4.020805332102288077, 42.55092418646378860, -150.0552959530000123 ) ) ;
#14144 = EDGE_CURVE ( 'NONE', #10397, #12619, #5398, .T. ) ;
#14145 = ORIENTED_EDGE ( 'NONE', *, *, #8148, .T. ) ;
#14146 =( NAMED_UNIT ( * ) PLANE_ANGLE_UNIT ( ) SI_UNIT ( $, .RADIAN. ) );
#14147 = ORIENTED_EDGE ( 'NONE', *, *, #2143, .F. ) ;
#14148 = DIRECTION ( 'NONE',  ( -1.000000000000000000, -5.988019148734350335E-18, 1.096099552913726042E-17 ) ) ;
#14149 = CARTESIAN_POINT ( 'NONE',  ( -11.11377970773875212, 36.98904460433607255, -140.6889018750557341 ) ) ;
#14150 = VERTEX_POINT ( 'NONE', #13435 ) ;
#14151 = VECTOR ( 'NONE', #2579, 1000.000000000000000 ) ;
#14152 = DIRECTION ( 'NONE',  ( 1.000000000000000000, 0.000000000000000000, -2.715621035259064790E-14 ) ) ;
#14153 = VECTOR ( 'NONE', #14880, 1000.000000000000114 ) ;
#14154 = DIRECTION ( 'NONE',  ( 1.457985068979999943E-12, 1.723073263340000007E-12, -1.000000000000000000 ) ) ;
#14155 = ORIENTED_EDGE ( 'NONE', *, *, #13601, .F. ) ;
#14156 = CARTESIAN_POINT ( 'NONE',  ( -13.82353779670000193, 34.78290842719999887, -141.1681162280000308 ) ) ;
#14157 = ORIENTED_EDGE ( 'NONE', *, *, #11548, .T. ) ;
#14158 = PLANE ( 'NONE',  #17744 ) ;
#14159 = ADVANCED_FACE ( 'NONE', ( #15109, #5947, #15237 ), #20359, .T. ) ;
#14160 = CARTESIAN_POINT ( 'NONE',  ( -22.00705883600000234, 37.05789963359999462, -148.1619053240000028 ) ) ;
#14161 = CARTESIAN_POINT ( 'NONE',  ( -15.26331651089999930, 39.75437292659999855, -147.8043400740000095 ) ) ;
#14162 = CARTESIAN_POINT ( 'NONE',  ( -29.32937220846275750, 40.41939957101679681, -140.7656299762288086 ) ) ;
#14163 = EDGE_LOOP ( 'NONE', ( #3993, #9242, #13955, #808 ) ) ;
#14164 = CARTESIAN_POINT ( 'NONE',  ( 22.27792782919999937, -15.32580087659999890, -145.0552959529999839 ) ) ;
#14165 = FACE_OUTER_BOUND ( 'NONE', #14818, .T. ) ;
#14166 = VECTOR ( 'NONE', #9758, 1000.000000000000000 ) ;
#14167 = PLANE ( 'NONE',  #15966 ) ;
#14168 = DIRECTION ( 'NONE',  ( -1.000000000000000000, 0.000000000000000000, 2.257120985840000117E-12 ) ) ;
#14169 = CARTESIAN_POINT ( 'NONE',  ( -32.50000000000000000, -62.58229784560000297, -140.5449657050000098 ) ) ;
#14170 = FACE_OUTER_BOUND ( 'NONE', #22371, .T. ) ;
#14171 = EDGE_CURVE ( 'NONE', #13781, #416, #11409, .T. ) ;
#14172 = EDGE_LOOP ( 'NONE', ( #18568, #17450, #2406, #18968 ) ) ;
#14173 = DIRECTION ( 'NONE',  ( 0.000000000000000000, -1.000000000000000000, 0.000000000000000000 ) ) ;
#14174 = CARTESIAN_POINT ( 'NONE',  ( -9.317785202249279308, -17.02322901197889848, -144.5552959530000123 ) ) ;
#14175 = CARTESIAN_POINT ( 'NONE',  ( 26.50000000000000000, -20.50000000000000000, -150.0552959529999839 ) ) ;
#14176 = CARTESIAN_POINT ( 'NONE',  ( -5.769798041881806228, 38.72966034773180866, -148.0785409402818118 ) ) ;
#14177 = CARTESIAN_POINT ( 'NONE',  ( 2.531727043930000143, -11.80034048859999807, -147.5552959529999839 ) ) ;
#14178 = EDGE_LOOP ( 'NONE', ( #1081, #1358, #10336, #21062 ) ) ;
#14179 = DIRECTION ( 'NONE',  ( 2.257144641399999941E-12, -8.049635416090000264E-35, 1.000000000000000000 ) ) ;
#14180 = EDGE_CURVE ( 'NONE', #23345, #23072, #3178, .T. ) ;
#14181 = PLANE ( 'NONE',  #13228 ) ;
#14182 = EDGE_LOOP ( 'NONE', ( #2467, #23030 ) ) ;
#14183 = CARTESIAN_POINT ( 'NONE',  ( -0.7500000000009999779, -50.00000000000000000, -149.5552959529999839 ) ) ;
#14184 = EDGE_LOOP ( 'NONE', ( #6161, #18175, #5394, #17398 ) ) ;
#14185 = CARTESIAN_POINT ( 'NONE',  ( 6.000000000160000013, 29.48610037779999971, -139.5552959529999839 ) ) ;
#14186 = EDGE_CURVE ( 'NONE', #258, #350, #16894, .T. ) ;
#14187 = DIRECTION ( 'NONE',  ( 1.000000000000000000, 0.000000000000000000, -4.510281037539699253E-12 ) ) ;
#14188 = EDGE_CURVE ( 'NONE', #20598, #19064, #3207, .T. ) ;
#14189 = CYLINDRICAL_SURFACE ( 'NONE', #8232, 1.500000000000001332 ) ;
#14190 = CARTESIAN_POINT ( 'NONE',  ( 7.243343564704193049, 36.18094154607518220, -141.6932697408899173 ) ) ;
#14191 = ORIENTED_EDGE ( 'NONE', *, *, #279, .T. ) ;
#14192 = CARTESIAN_POINT ( 'NONE',  ( -11.26413364454818122, 36.97109742514091124, -139.4278719022179018 ) ) ;
#14193 = FACE_OUTER_BOUND ( 'NONE', #19729, .T. ) ;
#14194 = ADVANCED_FACE ( 'NONE', ( #4517 ), #13912, .F. ) ;
#14195 = CYLINDRICAL_SURFACE ( 'NONE', #12443, 3.000000000000000000 ) ;
#14196 = FACE_OUTER_BOUND ( 'NONE', #408, .T. ) ;
#14197 = EDGE_CURVE ( 'NONE', #10168, #21289, #10086, .T. ) ;
#14198 = ORIENTED_EDGE ( 'NONE', *, *, #21706, .T. ) ;
#14199 =( GEOMETRIC_REPRESENTATION_CONTEXT ( 3 ) GLOBAL_UNCERTAINTY_ASSIGNED_CONTEXT ( ( #12542 ) ) GLOBAL_UNIT_ASSIGNED_CONTEXT ( ( #8176, #12458, #14018 ) ) REPRESENTATION_CONTEXT ( 'NONE', 'WORKASPACE' ) );
#14200 = CARTESIAN_POINT ( 'NONE',  ( 20.10234832544897543, 19.49999999999997513, -136.0552959530453450 ) ) ;
#14201 = AXIS2_PLACEMENT_3D ( 'NONE', #4223, #11461, #11335 ) ;
#14202 = B_SPLINE_CURVE_WITH_KNOTS ( 'NONE', 5,
 ( #2794, #10141, #17656, #19197, #8240, #3149, #2910, #17415, #15514, #21232, #10379, #15753 ),
 .UNSPECIFIED., .F., .F.,
 ( 6, 3, 3, 6 ),
 ( 0.000000000000000000, 4.390059406679999832, 8.746277600790000051, 13.07048654050000103 ),
 .UNSPECIFIED. ) ;
#14203 = ORIENTED_EDGE ( 'NONE', *, *, #11610, .T. ) ;
#14204 = CARTESIAN_POINT ( 'NONE',  ( -6.665693515917223699, 34.99563620361987404, -146.8660724163397333 ) ) ;
#14205 = CARTESIAN_POINT ( 'NONE',  ( -6.603585321229999749, -20.59801339440000234, -142.5552959529999839 ) ) ;
#14206 = CARTESIAN_POINT ( 'NONE',  ( -44.50000000000000000, 37.00000000000000000, -148.4460207619999892 ) ) ;
#14207 = EDGE_LOOP ( 'NONE', ( #3714, #15373, #22231, #1253 ) ) ;
#14208 = CARTESIAN_POINT ( 'NONE',  ( -5.579327536678420074, 37.66950319827602556, -140.5530665557081704 ) ) ;
#14209 = CARTESIAN_POINT ( 'NONE',  ( 17.44013884619999999, -20.67371738400000325, -145.5552959529999839 ) ) ;
#14210 = ORIENTED_EDGE ( 'NONE', *, *, #17684, .F. ) ;
#14211 = CARTESIAN_POINT ( 'NONE',  ( 20.50000000000000000, 19.50000000000000000, -150.5552959529999839 ) ) ;
#14212 = CARTESIAN_POINT ( 'NONE',  ( 20.50000000000000000, 19.50000000000000000, -150.0552959529999839 ) ) ;
#14213 = DIRECTION ( 'NONE',  ( 1.000000000000000000, 0.000000000000000000, -2.257144641399999941E-12 ) ) ;
#14214 = CARTESIAN_POINT ( 'NONE',  ( -21.35824191589999899, -32.00000000000000000, -144.8157682190000060 ) ) ;
#14215 = PLANE ( 'NONE',  #2508 ) ;
#14216 = CIRCLE ( 'NONE', #3211, 1.499999999999999556 ) ;
#14217 = EDGE_CURVE ( 'NONE', #5894, #9011, #1206, .T. ) ;
#14218 = CARTESIAN_POINT ( 'NONE',  ( -26.17844700321287377, 36.98132551455246642, -140.6351982806903607 ) ) ;
#14219 = CONTEXT_DEPENDENT_SHAPE_REPRESENTATION ( #17689, #22837 ) ;
#14220 = PLANE ( 'NONE',  #15075 ) ;
#14221 = CARTESIAN_POINT ( 'NONE',  ( -1.499999999960000219, 44.50000000000000000, -136.0552959530000123 ) ) ;
#14222 =( BOUNDED_CURVE ( )  B_SPLINE_CURVE ( 5, ( #19765, #21316, #19528, #3333, #15950, #7019 ),
 .UNSPECIFIED., .F., .F. ) 
 B_SPLINE_CURVE_WITH_KNOTS ( ( 6, 6 ),
 ( 1.570796326807921472, 3.141592653590000062 ),
 .UNSPECIFIED. ) 
 CURVE ( )  GEOMETRIC_REPRESENTATION_ITEM ( )  RATIONAL_B_SPLINE_CURVE ( ( 0.2500000000000000000, 0.2500000000016452395, 0.3000000000024678481, 0.4000000000032904457, 0.6000000000032904568, 1.000000000000000000 ) ) 
 REPRESENTATION_ITEM ( '' )  );
#14223 = CARTESIAN_POINT ( 'NONE',  ( -30.49999999990000177, 47.50000000000000000, -148.3052959529999839 ) ) ;
#14224 = ORIENTED_EDGE ( 'NONE', *, *, #23082, .F. ) ;
#14225 = CARTESIAN_POINT ( 'NONE',  ( 6.500000000000000000, 20.50000000000000000, -150.0552959529999839 ) ) ;
#14226 = UNCERTAINTY_MEASURE_WITH_UNIT (LENGTH_MEASURE( 1.000000000000000082E-05 ), #23332, 'distance_accuracy_value', 'NONE');
#14227 = VERTEX_POINT ( 'NONE', #22847 ) ;
#14228 =( LENGTH_UNIT ( ) NAMED_UNIT ( * ) SI_UNIT ( .MILLI., .METRE. ) );
#14229 = ORIENTED_EDGE ( 'NONE', *, *, #6146, .T. ) ;
#14230 = DIRECTION ( 'NONE',  ( 2.688820921349999492E-17, -1.000000000000000000, -6.069065783950000909E-29 ) ) ;
#14231 = CARTESIAN_POINT ( 'NONE',  ( -28.14233742207320788, 35.42069160767093194, -140.2329357297371359 ) ) ;
#14232 = ORIENTED_EDGE ( 'NONE', *, *, #20447, .T. ) ;
#14233 = LINE ( 'NONE', #15342, #14847 ) ;
#14234 = ORIENTED_EDGE ( 'NONE', *, *, #12141, .T. ) ;
#14235 = VECTOR ( 'NONE', #16436, 1000.000000000000227 ) ;
#14236 = CARTESIAN_POINT ( 'NONE',  ( 23.28094649259046989, 39.42349012525005492, -136.0552959530525641 ) ) ;
#14237 = CARTESIAN_POINT ( 'NONE',  ( -19.28609856400827738, 34.66429844319404197, -140.9609051181238044 ) ) ;
#14238 = LINE ( 'NONE', #16021, #15696 ) ;
#14239 = CARTESIAN_POINT ( 'NONE',  ( -0.7499999998570000548, 41.50000000000000000, -146.5552959529999839 ) ) ;
#14240 = EDGE_LOOP ( 'NONE', ( #11161, #15060 ) ) ;
#14241 = CARTESIAN_POINT ( 'NONE',  ( 10.50000000010000001, 16.50000000000000000, -150.5552959529999839 ) ) ;
#14242 = EDGE_LOOP ( 'NONE', ( #6375, #8968, #7880, #260 ) ) ;
#14243 = CARTESIAN_POINT ( 'NONE',  ( 9.962781063757809363, 36.60796380593278343, -141.5783597023373943 ) ) ;
#14244 = EDGE_CURVE ( 'NONE', #5226, #1779, #17608, .T. ) ;
#14245 = DIRECTION ( 'NONE',  ( 1.000000000000000000, 0.000000000000000000, -2.256131789327550371E-12 ) ) ;
#14246 = CARTESIAN_POINT ( 'NONE',  ( -21.35824191589999899, -4.000000000000000000, -146.2257682199999920 ) ) ;
#14247 = EDGE_LOOP ( 'NONE', ( #13995, #698, #10067, #9778, #15170 ) ) ;
#14248 = CARTESIAN_POINT ( 'NONE',  ( -18.35824191589999899, -1.500000000000000000, -144.8157682190000060 ) ) ;
#14249 = ORIENTED_EDGE ( 'NONE', *, *, #4950, .T. ) ;
#14250 = AXIS2_PLACEMENT_3D ( 'NONE', #10396, #17670, #8605 ) ;
#14251 = DIRECTION ( 'NONE',  ( 1.000000000000000000, 0.000000000000000000, -2.257171095940000041E-12 ) ) ;
#14252 = LINE ( 'NONE', #16038, #10469 ) ;
#14253 = ORIENTED_EDGE ( 'NONE', *, *, #19463, .F. ) ;
#14254 = CARTESIAN_POINT ( 'NONE',  ( -11.19806794730000021, 41.07225940149999843, -141.8826665010000170 ) ) ;
#14255 = ORIENTED_EDGE ( 'NONE', *, *, #16811, .F. ) ;
#14256 = CARTESIAN_POINT ( 'NONE',  ( -15.86060558933779419, 39.62525409245568397, -147.5113276022380830 ) ) ;
#14257 = CARTESIAN_POINT ( 'NONE',  ( -5.499999999960006214, 44.76520911280675818, -136.0552959529875920 ) ) ;
#14258 = ORIENTED_EDGE ( 'NONE', *, *, #18363, .T. ) ;
#14259 = SURFACE_SIDE_STYLE ('',( #16045 ) ) ;
#14260 = VERTEX_POINT ( 'NONE', #8308 ) ;
#14261 = CARTESIAN_POINT ( 'NONE',  ( -25.95437585238067868, 39.65968214927003288, -140.4458241779535967 ) ) ;
#14262 = DIRECTION ( 'NONE',  ( 2.257083409060000051E-12, 0.000000000000000000, 1.000000000000000000 ) ) ;
#14263 = VERTEX_POINT ( 'NONE', #17718 ) ;
#14264 = CARTESIAN_POINT ( 'NONE',  ( 4.999999999879999990, -4.000000000000000000, -135.2552959529999725 ) ) ;
#14265 = DIRECTION ( 'NONE',  ( -0.9753087663813413410, 0.2208456705930775810, 8.936242978303132921E-12 ) ) ;
#14266 = ORIENTED_EDGE ( 'NONE', *, *, #9640, .F. ) ;
#14267 = CARTESIAN_POINT ( 'NONE',  ( -2.489991676560021627, 46.24652334969350420, -150.0552959530000408 ) ) ;
#14268 = AXIS2_PLACEMENT_3D ( 'NONE', #18485, #7191, #2200 ) ;
#14269 = EDGE_CURVE ( 'NONE', #17671, #11516, #21183, .T. ) ;
#14270 = EDGE_CURVE ( 'NONE', #21310, #322, #15583, .T. ) ;
#14271 = EDGE_LOOP ( 'NONE', ( #2709, #5189 ) ) ;
#14272 = CARTESIAN_POINT ( 'NONE',  ( -2.203055323360000095, -15.74846988260000025, -143.5552959529999839 ) ) ;
#14273 = CARTESIAN_POINT ( 'NONE',  ( -20.60824191589811605, -4.000000000000000000, -146.3157682190056335 ) ) ;
#14274 = CARTESIAN_POINT ( 'NONE',  ( -15.00140173387118026, 40.20535686067567838, -145.8913236318710176 ) ) ;
#14275 = CARTESIAN_POINT ( 'NONE',  ( -29.13601448249999848, 36.98639052360000079, -140.5419328609999923 ) ) ;
#14276 = ORIENTED_EDGE ( 'NONE', *, *, #9433, .F. ) ;
#14277 = CARTESIAN_POINT ( 'NONE',  ( -0.7600837003953544446, 18.55411937531343014, -136.0552959529982502 ) ) ;
#14278 = DIRECTION ( 'NONE',  ( 0.000000000000000000, -1.000000000000000000, 0.000000000000000000 ) ) ;
#14279 = CARTESIAN_POINT ( 'NONE',  ( -9.282104535860000283, -16.71402168319999859, -145.5552959529999839 ) ) ;
#14280 = DIRECTION ( 'NONE',  ( 0.000000000000000000, -1.000000000000000000, 0.000000000000000000 ) ) ;
#14281 = CARTESIAN_POINT ( 'NONE',  ( -4.499999999929999994, 42.50000000000000000, -138.0552959530000123 ) ) ;
#14282 = DIRECTION ( 'NONE',  ( 0.000000000000000000, -1.000000000000000000, 0.000000000000000000 ) ) ;
#14283 = AXIS2_PLACEMENT_3D ( 'NONE', #18671, #7823, #9485 ) ;
#14284 = AXIS2_PLACEMENT_3D ( 'NONE', #15524, #13745, #2345 ) ;
#14285 = ORIENTED_EDGE ( 'NONE', *, *, #5874, .F. ) ;
#14286 = DIRECTION ( 'NONE',  ( 1.000000000000000000, -5.094701932209999624E-24, -2.257144641399999941E-12 ) ) ;
#14287 = CARTESIAN_POINT ( 'NONE',  ( 25.50000000000000000, 19.50000000000000000, -150.5552959529999839 ) ) ;
#14288 = PLANE ( 'NONE',  #4908 ) ;
#14289 = CARTESIAN_POINT ( 'NONE',  ( -6.033650297970000409, 36.94170754819999303, -147.9652040070000112 ) ) ;
#14290 = DIRECTION ( 'NONE',  ( 0.000000000000000000, -1.000000000000000000, 3.568879590630000244E-13 ) ) ;
#14291 = CARTESIAN_POINT ( 'NONE',  ( 19.04211518520000013, 51.50000000000000000, -149.5552959529999839 ) ) ;
#14292 = ORIENTED_EDGE ( 'NONE', *, *, #1957, .F. ) ;
#14293 = DIRECTION ( 'NONE',  ( 0.000000000000000000, 1.000000000000000000, 0.000000000000000000 ) ) ;
#14294 = CARTESIAN_POINT ( 'NONE',  ( -9.157754307290000284, -15.75963164970000108, -147.5552959529999839 ) ) ;
#14295 = EDGE_LOOP ( 'NONE', ( #6724, #4650, #12924, #10440 ) ) ;
#14296 = VECTOR ( 'NONE', #15464, 1000.000000000000000 ) ;
#14297 = EDGE_CURVE ( 'NONE', #10668, #12077, #4991, .T. ) ;
#14298 = CARTESIAN_POINT ( 'NONE',  ( -2.121568318600000058, -15.32705806070000243, -144.5552959529999839 ) ) ;
#14299 = ORIENTED_EDGE ( 'NONE', *, *, #23215, .T. ) ;
#14300 = DIRECTION ( 'NONE',  ( 0.000000000000000000, 0.000000000000000000, 1.000000000000000000 ) ) ;
#14301 = CARTESIAN_POINT ( 'NONE',  ( -28.90798551733967869, 37.01360947636671739, -139.5686590453834128 ) ) ;
#14302 = DIRECTION ( 'NONE',  ( 0.000000000000000000, 1.000000000000000000, 0.000000000000000000 ) ) ;
#14303 = CARTESIAN_POINT ( 'NONE',  ( 7.930184371052885872, 38.38757070224898627, -141.9757830863086667 ) ) ;
#14304 = ORIENTED_EDGE ( 'NONE', *, *, #18111, .T. ) ;
#14305 = CARTESIAN_POINT ( 'NONE',  ( -11.10890527080962009, 34.84141842887415663, -140.9538660576732241 ) ) ;
#14306 = DIRECTION ( 'NONE',  ( 1.000000000000000000, 0.000000000000000000, 0.000000000000000000 ) ) ;
#14307 = CARTESIAN_POINT ( 'NONE',  ( -8.396783337457932817, 40.57449494537098644, -144.4531261594902958 ) ) ;
#14308 = CARTESIAN_POINT ( 'NONE',  ( 3.736991614122307848, -33.86279581096970759, -136.0552959530084536 ) ) ;
#14309 = EDGE_CURVE ( 'NONE', #22853, #12372, #6648, .T. ) ;
#14310 = ORIENTED_EDGE ( 'NONE', *, *, #50, .F. ) ;
#14311 = CARTESIAN_POINT ( 'NONE',  ( 6.750000000030000002, -33.75000000000000000, -137.0552959530000123 ) ) ;
#14312 = ORIENTED_EDGE ( 'NONE', *, *, #21099, .F. ) ;
#14313 = AXIS2_PLACEMENT_3D ( 'NONE', #7312, #18375, #2087 ) ;
#14314 = CARTESIAN_POINT ( 'NONE',  ( -7.486908230310626244, 37.06387187510053849, -140.3212062627006560 ) ) ;
#14315 = CARTESIAN_POINT ( 'NONE',  ( 31.64594224149999846, -40.56768785850000825, -149.5552959529999839 ) ) ;
#14316 = CARTESIAN_POINT ( 'NONE',  ( -4.576286989381322279, 23.28076054106353965, -136.0552959529896668 ) ) ;
#14317 = EDGE_CURVE ( 'NONE', #6977, #10222, #1429, .T. ) ;
#14318 = ORIENTED_EDGE ( 'NONE', *, *, #17048, .T. ) ;
#14319 = PLANE ( 'NONE',  #10629 ) ;
#14320 = LINE ( 'NONE', #3618, #7961 ) ;
#14321 = ADVANCED_FACE ( 'NONE', ( #8540 ), #11881, .T. ) ;
#14322 = VERTEX_POINT ( 'NONE', #15703 ) ;
#14323 = PLANE ( 'NONE',  #4199 ) ;
#14324 = EDGE_CURVE ( 'NONE', #9455, #2716, #22717, .T. ) ;
#14325 = EDGE_CURVE ( 'NONE', #10651, #18413, #15651, .T. ) ;
#14326 = DIRECTION ( 'NONE',  ( 1.000000000000000000, 0.000000000000000000, -2.267228047249999995E-12 ) ) ;
#14327 = FACE_OUTER_BOUND ( 'NONE', #12335, .T. ) ;
#14328 = DIRECTION ( 'NONE',  ( -4.510774274160000731E-12, 1.321907670990000086E-13, -1.000000000000000000 ) ) ;
#14329 = AXIS2_PLACEMENT_3D ( 'NONE', #4236, #556, #22091 ) ;
#14330 = CARTESIAN_POINT ( 'NONE',  ( -9.434278515689999978, -18.41834002140000237, -147.5552959529999839 ) ) ;
#14331 = VECTOR ( 'NONE', #9743, 1000.000000000000000 ) ;
#14332 = LINE ( 'NONE', #19927, #9750 ) ;
#14333 = DIRECTION ( 'NONE',  ( -2.257157423930000049E-12, 0.000000000000000000, -1.000000000000000000 ) ) ;
#14334 = CARTESIAN_POINT ( 'NONE',  ( -35.33948162989999986, 16.82262754929999815, -144.5552959529999839 ) ) ;
#14335 = DIRECTION ( 'NONE',  ( 0.000000000000000000, 1.000000000000000000, 0.000000000000000000 ) ) ;
#14336 = ADVANCED_FACE ( 'NONE', ( #12117, #9973, #958 ), #2976, .T. ) ;
#14337 = EDGE_LOOP ( 'NONE', ( #1434, #6539, #3143, #2333, #14134, #9344, #11840, #14304, #11929, #3965, #20827, #6168, #12976, #8182, #11572 ) ) ;
#14338 = VERTEX_POINT ( 'NONE', #6413 ) ;
#14339 = ORIENTED_EDGE ( 'NONE', *, *, #6417, .T. ) ;
#14340 = CARTESIAN_POINT ( 'NONE',  ( -16.06433926788437461, 35.52312188426208905, -147.3204108562227646 ) ) ;
#14341 = FACE_OUTER_BOUND ( 'NONE', #1164, .T. ) ;
#14342 = DIRECTION ( 'NONE',  ( -2.257198259660000092E-12, 0.000000000000000000, -1.000000000000000000 ) ) ;
#14343 = CARTESIAN_POINT ( 'NONE',  ( -6.601136089949999786, -20.10368962670000315, -143.5552959529999839 ) ) ;
#14344 = AXIS2_PLACEMENT_3D ( 'NONE', #21340, #21696, #5033 ) ;
#14345 = EDGE_CURVE ( 'NONE', #10310, #11694, #13675, .T. ) ;
#14346 = ORIENTED_EDGE ( 'NONE', *, *, #8827, .T. ) ;
#14347 = CARTESIAN_POINT ( 'NONE',  ( -5.098183173407200286, 20.66060904161428269, -150.0552959529999839 ) ) ;
#14348 = CARTESIAN_POINT ( 'NONE',  ( -19.68769410165050715, 36.28218526682968559, -140.6463262768891127 ) ) ;
#14349 = ADVANCED_FACE ( 'NONE', ( #3095 ), #5216, .T. ) ;
#14350 = AXIS2_PLACEMENT_3D ( 'NONE', #6050, #13300, #4272 ) ;
#14351 = CARTESIAN_POINT ( 'NONE',  ( -12.32040252380945589, 37.67168662422751169, -147.4262574636698844 ) ) ;
#14352 = DIRECTION ( 'NONE',  ( 4.569805223421110083E-12, 0.000000000000000000, 1.000000000000000000 ) ) ;
#14353 = ORIENTED_EDGE ( 'NONE', *, *, #23188, .T. ) ;
#14354 = CARTESIAN_POINT ( 'NONE',  ( 5.631397321050000571, -17.85059010000000157, -147.5552959529999839 ) ) ;
#14355 = ADVANCED_FACE ( 'NONE', ( #18312 ), #21778, .T. ) ;
#14356 = APPLICATION_CONTEXT ( 'automotive_design' ) ;
#14357 = ORIENTED_EDGE ( 'NONE', *, *, #21172, .F. ) ;
#14358 = CARTESIAN_POINT ( 'NONE',  ( 9.247017358121205177, 35.69898662692506264, -141.9204103852138417 ) ) ;
#14359 = CARTESIAN_POINT ( 'NONE',  ( -6.657076963140000636, -20.13603737529999904, -145.0552959529999839 ) ) ;
#14360 = CARTESIAN_POINT ( 'NONE',  ( -33.36626399469999882, 26.50000000000000000, -138.5552959529999839 ) ) ;
#14361 = VERTEX_POINT ( 'NONE', #10790 ) ;
#14362 = VECTOR ( 'NONE', #11077, 1000.000000000000000 ) ;
#14363 = CARTESIAN_POINT ( 'NONE',  ( 2.016283561950000358, -13.16498300129999954, -142.5552959529999839 ) ) ;
#14364 = VECTOR ( 'NONE', #11648, 1000.000000000000000 ) ;
#14365 = VERTEX_POINT ( 'NONE', #3318 ) ;
#14366 = CARTESIAN_POINT ( 'NONE',  ( -18.90246017573007720, 37.04541408823331494, -147.4848489023210050 ) ) ;
#14367 = DIRECTION ( 'NONE',  ( 0.000000000000000000, 1.000000000000000000, 0.000000000000000000 ) ) ;
#14368 = ORIENTED_EDGE ( 'NONE', *, *, #22815, .F. ) ;
#14369 = DIRECTION ( 'NONE',  ( 5.094701932209999624E-24, 1.000000000000000000, -1.149947916579999802E-35 ) ) ;
#14370 = VERTEX_POINT ( 'NONE', #10676 ) ;
#14371 = DIRECTION ( 'NONE',  ( -1.000000000000000000, 0.000000000000000000, 0.000000000000000000 ) ) ;
#14372 = PLANE ( 'NONE',  #20919 ) ;
#14373 = EDGE_LOOP ( 'NONE', ( #6745, #20803, #22564, #6890, #1950, #22968, #19152, #11878 ) ) ;
#14374 = DIRECTION ( 'NONE',  ( 1.000000000000000000, 0.000000000000000000, 0.000000000000000000 ) ) ;
#14375 = EDGE_CURVE ( 'NONE', #16830, #12039, #120, .T. ) ;
#14376 = ORIENTED_EDGE ( 'NONE', *, *, #21351, .F. ) ;
#14377 = CARTESIAN_POINT ( 'NONE',  ( -26.39607007120000048, 36.95534867429999792, -140.3840478969999879 ) ) ;
#14378 = ADVANCED_FACE ( 'NONE', ( #7360 ), #21417, .T. ) ;
#14379 = CARTESIAN_POINT ( 'NONE',  ( 2.531727043930000143, -11.80034048859999807, -147.5552959529999839 ) ) ;
#14380 = ORIENTED_EDGE ( 'NONE', *, *, #7416, .T. ) ;
#14381 = CARTESIAN_POINT ( 'NONE',  ( -18.35824191589999899, -34.50000000000000000, -142.9407682190000060 ) ) ;
#14382 = CARTESIAN_POINT ( 'NONE',  ( -10.69115198329542160, 37.03949207291182688, -140.6562969416297335 ) ) ;
#14383 = CIRCLE ( 'NONE', #19322, 1.500000000000001332 ) ;
#14384 = CARTESIAN_POINT ( 'NONE',  ( -5.499999999959999997, 44.50000000000000000, -136.0552959530000123 ) ) ;
#14385 = ORIENTED_EDGE ( 'NONE', *, *, #10838, .F. ) ;
#14386 = AXIS2_PLACEMENT_3D ( 'NONE', #12570, #21280, #8758 ) ;
#14387 = CARTESIAN_POINT ( 'NONE',  ( -16.72278394150000125, 36.31586521340000218, -140.5063707120000061 ) ) ;
#14388 = ORIENTED_EDGE ( 'NONE', *, *, #1675, .F. ) ;
#14389 = CARTESIAN_POINT ( 'NONE',  ( 10.50000000020000002, 16.50000000000000000, -136.5552959530000123 ) ) ;
#14390 = CARTESIAN_POINT ( 'NONE',  ( -9.334216945200001447, -17.19633444960000190, -145.5552959529999839 ) ) ;
#14391 = DIRECTION ( 'NONE',  ( 0.000000000000000000, -1.000000000000000000, -2.765629237170000203E-27 ) ) ;
#14392 = CARTESIAN_POINT ( 'NONE',  ( -29.04280990185221967, 38.86145750698325685, -140.9282040248405110 ) ) ;
#14393 = ORIENTED_EDGE ( 'NONE', *, *, #2786, .T. ) ;
#14394 = CARTESIAN_POINT ( 'NONE',  ( 16.07620488043449569, -22.91638164385598841, -147.5552959530484429 ) ) ;
#14395 = CARTESIAN_POINT ( 'NONE',  ( -25.38678224712056775, 37.07582353396835373, -140.0279244692600855 ) ) ;
#14396 = AXIS2_PLACEMENT_3D ( 'NONE', #19266, #17250, #8188 ) ;
#14397 = DIRECTION ( 'NONE',  ( 2.257144641399999941E-12, -8.049635416090000264E-35, 1.000000000000000000 ) ) ;
#14398 = CYLINDRICAL_SURFACE ( 'NONE', #10531, 1.000000000000001332 ) ;
#14399 = DIRECTION ( 'NONE',  ( 1.000000000000000000, 0.000000000000000000, 0.000000000000000000 ) ) ;
#14400 = CARTESIAN_POINT ( 'NONE',  ( -34.50000000000000000, 37.00000000000000000, -150.5552959529999839 ) ) ;
#14401 = AXIS2_PLACEMENT_3D ( 'NONE', #8500, #21932, #3721 ) ;
#14402 = ORIENTED_EDGE ( 'NONE', *, *, #20421, .T. ) ;
#14403 = ADVANCED_FACE ( 'NONE', ( #8478 ), #9248, .T. ) ;
#14404 = LINE ( 'NONE', #21681, #19828 ) ;
#14405 = VECTOR ( 'NONE', #9849, 999.9999999999998863 ) ;
#14406 = CARTESIAN_POINT ( 'NONE',  ( 15.59498359470000040, -26.23371093219999750, -148.5552959529999839 ) ) ;
#14407 = ADVANCED_FACE ( 'NONE', ( #8893 ), #23311, .T. ) ;
#14408 = AXIS2_PLACEMENT_3D ( 'NONE', #15931, #23196, #11755 ) ;
#14409 = CARTESIAN_POINT ( 'NONE',  ( -13.71246964740000074, 35.06639867129999999, -139.8243480419999685 ) ) ;
#14410 = CARTESIAN_POINT ( 'NONE',  ( -5.059418532210888664, 38.95414396229264042, -139.6466485215420619 ) ) ;
#14411 = EDGE_CURVE ( 'NONE', #19876, #6873, #6883, .T. ) ;
#14412 = CARTESIAN_POINT ( 'NONE',  ( -14.80365045915063327, -44.50000000000000711, -136.0552959530004387 ) ) ;
#14413 = VERTEX_POINT ( 'NONE', #11036 ) ;
#14414 = CARTESIAN_POINT ( 'NONE',  ( 9.683200060760002614, -20.63250393952945316, -148.5552959529999839 ) ) ;
#14415 = FACE_OUTER_BOUND ( 'NONE', #6529, .T. ) ;
#14416 = ORIENTED_EDGE ( 'NONE', *, *, #1639, .T. ) ;
#14417 = VECTOR ( 'NONE', #17748, 1000.000000000000000 ) ;
#14418 = CARTESIAN_POINT ( 'NONE',  ( 25.50000000000000000, 22.50000000000000000, -136.0552959530000123 ) ) ;
#14419 = ORIENTED_EDGE ( 'NONE', *, *, #11641, .T. ) ;
#14420 = VECTOR ( 'NONE', #6263, 1000.000000000000114 ) ;
#14421 = VECTOR ( 'NONE', #16257, 1000.000000000000000 ) ;
#14422 = DIRECTION ( 'NONE',  ( -1.000000000000000000, 0.000000000000000000, 0.000000000000000000 ) ) ;
#14423 = CARTESIAN_POINT ( 'NONE',  ( -29.97886196652672197, 40.49728245963383699, -142.7481031354987238 ) ) ;
#14424 = CIRCLE ( 'NONE', #16312, 3.000000000000000888 ) ;
#14425 = FACE_OUTER_BOUND ( 'NONE', #21779, .T. ) ;
#14426 = CARTESIAN_POINT ( 'NONE',  ( 7.456043044519751639, 38.07711648188232800, -141.7992203782033300 ) ) ;
#14427 = ORIENTED_EDGE ( 'NONE', *, *, #7168, .F. ) ;
#14428 = CARTESIAN_POINT ( 'NONE',  ( -10.58679693489213491, 34.36322230824750079, -140.1414225335838921 ) ) ;
#14429 = CARTESIAN_POINT ( 'NONE',  ( -18.90938373568686259, 34.33541876391318226, -147.9661085319850713 ) ) ;
#14430 = CARTESIAN_POINT ( 'NONE',  ( -9.771488485234659294, 38.65068379629019546, -147.6127673914778029 ) ) ;
#14431 = LINE ( 'NONE', #17757, #2720 ) ;
#14432 = ORIENTED_EDGE ( 'NONE', *, *, #18801, .T. ) ;
#14433 = DIRECTION ( 'NONE',  ( -1.000000000000000000, -3.994014902950000436E-29, 0.000000000000000000 ) ) ;
#14434 = EDGE_LOOP ( 'NONE', ( #2392, #12315, #15025, #9803 ) ) ;
#14435 = DIRECTION ( 'NONE',  ( -0.9892101392001054760, 0.1465035852930155480, 4.471739159800472250E-12 ) ) ;
#14436 = LINE ( 'NONE', #20496, #463 ) ;
#14437 = EDGE_CURVE ( 'NONE', #11235, #18574, #23138, .T. ) ;
#14438 = LINE ( 'NONE', #23366, #5092 ) ;
#14439 = AXIS2_PLACEMENT_3D ( 'NONE', #6946, #21829, #8836 ) ;
#14440 = VECTOR ( 'NONE', #5400, 999.9999999999998863 ) ;
#14441 = EDGE_LOOP ( 'NONE', ( #15336, #13801, #7008, #22899 ) ) ;
#14442 = VECTOR ( 'NONE', #8448, 1000.000000000000000 ) ;
#14443 = PLANE ( 'NONE',  #772 ) ;
#14444 = AXIS2_PLACEMENT_3D ( 'NONE', #18071, #9127, #16406 ) ;
#14445 = CARTESIAN_POINT ( 'NONE',  ( -2.500000000000000000, 34.00000000000000000, -150.5552959529999839 ) ) ;
#14446 = VERTEX_POINT ( 'NONE', #1786 ) ;
#14447 = LINE ( 'NONE', #19569, #22434 ) ;
#14448 = PRODUCT_DEFINITION ( 'UNKNOWN', '', #3943, #12069 ) ;
#14449 = ADVANCED_FACE ( 'NONE', ( #9006 ), #5346, .F. ) ;
#14450 = DIRECTION ( 'NONE',  ( 1.000000000000000000, 0.000000000000000000, -2.257120985840000117E-12 ) ) ;
#14451 = DIRECTION ( 'NONE',  ( 0.000000000000000000, 0.000000000000000000, 1.000000000000000000 ) ) ;
#14452 = CARTESIAN_POINT ( 'NONE',  ( -8.594304764359998572, -10.75357442870000035, -145.5552959529999839 ) ) ;
#14453 = PLANE ( 'NONE',  #18830 ) ;
#14454 = DIRECTION ( 'NONE',  ( 4.430318231639999944E-12, -6.100259101500000139E-13, 1.000000000000000000 ) ) ;
#14455 = APPLICATION_PROTOCOL_DEFINITION ( 'draft international standard', 'automotive_design', 1998, #18899 ) ;
#14456 = CARTESIAN_POINT ( 'NONE',  ( 17.33131581010000133, -22.98361965280000163, -146.5552959529999839 ) ) ;
#14457 = AXIS2_PLACEMENT_3D ( 'NONE', #10701, #7266, #3583 ) ;
#14458 = DIRECTION ( 'NONE',  ( 1.000000000000000000, 0.000000000000000000, 0.000000000000000000 ) ) ;
#14459 = AXIS2_PLACEMENT_3D ( 'NONE', #12558, #19835, #10523 ) ;
#14460 = EDGE_CURVE ( 'NONE', #19147, #18032, #19974, .T. ) ;
#14461 = CARTESIAN_POINT ( 'NONE',  ( -21.35824191589999899, -32.00000000000000000, -146.3157682190000060 ) ) ;
#14462 = ORIENTED_EDGE ( 'NONE', *, *, #10734, .F. ) ;
#14463 = UNCERTAINTY_MEASURE_WITH_UNIT (LENGTH_MEASURE( 1.000000000000000082E-05 ), #22385, 'distance_accuracy_value', 'NONE');
#14464 = ORIENTED_EDGE ( 'NONE', *, *, #6683, .F. ) ;
#14465 = ORIENTED_EDGE ( 'NONE', *, *, #15044, .T. ) ;
#14466 = LINE ( 'NONE', #21734, #20118 ) ;
#14467 = LINE ( 'NONE', #8856, #825 ) ;
#14468 = ORIENTED_EDGE ( 'NONE', *, *, #7235, .T. ) ;
#14469 = EDGE_CURVE ( 'NONE', #11485, #6588, #5571, .T. ) ;
#14470 = DIRECTION ( 'NONE',  ( -0.1000233216789610108, -0.9949850929136109245, 3.559993607998610461E-13 ) ) ;
#14471 = ORIENTED_EDGE ( 'NONE', *, *, #13973, .F. ) ;
#14472 = CARTESIAN_POINT ( 'NONE',  ( -4.880807653193565798, 20.98537695657093138, -150.0552959529999839 ) ) ;
#14473 = CARTESIAN_POINT ( 'NONE',  ( -19.32129348605712593, 33.83991419265531420, -142.3697286030541704 ) ) ;
#14474 = CARTESIAN_POINT ( 'NONE',  ( -12.66714788137640113, 37.75265353618991782, -147.6129237412843906 ) ) ;
#14475 = DIRECTION ( 'NONE',  ( 0.000000000000000000, 0.000000000000000000, -1.000000000000000000 ) ) ;
#14476 = AXIS2_PLACEMENT_3D ( 'NONE', #14279, #7136, #12720 ) ;
#14477 = ORIENTED_EDGE ( 'NONE', *, *, #770, .F. ) ;
#14478 = AXIS2_PLACEMENT_3D ( 'NONE', #12171, #13725, #15633 ) ;
#14479 = DIRECTION ( 'NONE',  ( 2.257144641397284947E-12, 2.714590281723094849E-24, 1.000000000000000000 ) ) ;
#14480 = ORIENTED_EDGE ( 'NONE', *, *, #19894, .T. ) ;
#14481 = EDGE_CURVE ( 'NONE', #14876, #15664, #15148, .T. ) ;
#14482 = CARTESIAN_POINT ( 'NONE',  ( 9.451164963400199071, 35.83966787717029234, -141.8404982676872237 ) ) ;
#14483 = EDGE_CURVE ( 'NONE', #11594, #10244, #10554, .T. ) ;
#14484 = FACE_OUTER_BOUND ( 'NONE', #21418, .T. ) ;
#14485 = DIRECTION ( 'NONE',  ( -1.527666881879999979E-13, -8.171241461240000022E-13, -1.000000000000000000 ) ) ;
#14486 = VERTEX_POINT ( 'NONE', #14384 ) ;
#14487 = EDGE_CURVE ( 'NONE', #824, #19147, #1908, .T. ) ;
#14488 = ADVANCED_FACE ( 'NONE', ( #14619 ), #21886, .F. ) ;
#14489 = DIRECTION ( 'NONE',  ( -0.000000000000000000, 1.000000000000000000, 0.000000000000000000 ) ) ;
#14490 = ORIENTED_EDGE ( 'NONE', *, *, #3446, .F. ) ;
#14491 = DIRECTION ( 'NONE',  ( 0.7071067811866730279, 0.3390050494208429743, 0.6205445805637129775 ) ) ;
#14492 = AXIS2_PLACEMENT_3D ( 'NONE', #21399, #21635, #1300 ) ;
#14493 = FACE_OUTER_BOUND ( 'NONE', #20646, .T. ) ;
#14494 = AXIS2_PLACEMENT_3D ( 'NONE', #5975, #7641, #13227 ) ;
#14495 = EDGE_CURVE ( 'NONE', #13536, #1424, #11148, .T. ) ;
#14496 = VERTEX_POINT ( 'NONE', #4024 ) ;
#14497 = CARTESIAN_POINT ( 'NONE',  ( 25.50000000000000000, 19.50000000000000000, -151.0552959529999839 ) ) ;
#14498 = ORIENTED_EDGE ( 'NONE', *, *, #10349, .T. ) ;
#14499 = CARTESIAN_POINT ( 'NONE',  ( -15.36599175854349930, 37.73046438849700479, -147.5598381917543804 ) ) ;
#14500 = EDGE_CURVE ( 'NONE', #6268, #4735, #11255, .T. ) ;
#14501 = DIRECTION ( 'NONE',  ( -0.6459422414661291079, 0.7633862853691523176, -2.273736754430455399E-12 ) ) ;
#14502 = ORIENTED_EDGE ( 'NONE', *, *, #20666, .F. ) ;
#14503 = CARTESIAN_POINT ( 'NONE',  ( 0.000000000000000000, 0.000000000000000000, 0.000000000000000000 ) ) ;
#14504 = ORIENTED_EDGE ( 'NONE', *, *, #7878, .T. ) ;
#14505 = CARTESIAN_POINT ( 'NONE',  ( -1.844824604560000081, -14.10750774809999974, -147.5552959529999839 ) ) ;
#14506 = DIRECTION ( 'NONE',  ( 4.430318231639999944E-12, -6.100259101500000139E-13, 1.000000000000000000 ) ) ;
#14507 = ORIENTED_EDGE ( 'NONE', *, *, #10463, .F. ) ;
#14508 = PLANE ( 'NONE',  #14444 ) ;
#14509 =( BOUNDED_CURVE ( )  B_SPLINE_CURVE ( 5, ( #6317, #22740, #8213, #6670, #11779, #12142 ),
 .UNSPECIFIED., .F., .F. ) 
 B_SPLINE_CURVE_WITH_KNOTS ( ( 6, 6 ),
 ( 0.000000000000000000, 1.570796326447242430 ),
 .UNSPECIFIED. ) 
 CURVE ( )  GEOMETRIC_REPRESENTATION_ITEM ( )  RATIONAL_B_SPLINE_CURVE ( ( 1.000000000000000000, 0.6000000000885556961, 0.4000000000885557405, 0.3000000000664168054, 0.2500000000442779147, 0.2500000000000000000 ) ) 
 REPRESENTATION_ITEM ( '' )  );
#14510 = DIRECTION ( 'NONE',  ( 1.526468026909999897E-13, 8.159623473500000156E-13, 1.000000000000000000 ) ) ;
#14511 = DIRECTION ( 'NONE',  ( 0.7633862853691523176, 0.6459422414661291079, 0.000000000000000000 ) ) ;
#14512 = ORIENTED_EDGE ( 'NONE', *, *, #21780, .T. ) ;
#14513 = CARTESIAN_POINT ( 'NONE',  ( -16.20147620269999678, 33.40528963979999588, -143.4816615020000086 ) ) ;
#14514 = CIRCLE ( 'NONE', #4241, 1.000000000000000888 ) ;
#14515 = AXIS2_PLACEMENT_3D ( 'NONE', #21085, #14286, #3462 ) ;
#14516 = FACE_OUTER_BOUND ( 'NONE', #8824, .T. ) ;
#14517 = VERTEX_POINT ( 'NONE', #11492 ) ;
#14518 = CARTESIAN_POINT ( 'NONE',  ( 25.96278831570000278, -46.03148680980000051, -150.0552959529999839 ) ) ;
#14519 = CARTESIAN_POINT ( 'NONE',  ( -10.65913935279999869, 37.04331329920000115, -139.7140392919999954 ) ) ;
#14520 = ADVANCED_FACE ( 'NONE', ( #575 ), #336, .F. ) ;
#14521 = CARTESIAN_POINT ( 'NONE',  ( -16.74301326758274300, 39.28355396474279360, -140.9617246865330173 ) ) ;
#14522 = LINE ( 'NONE', #22007, #18226 ) ;
#14523 = EDGE_LOOP ( 'NONE', ( #5672, #6606, #15922, #5787 ) ) ;
#14524 = LINE ( 'NONE', #14164, #10535 ) ;
#14525 = LINE ( 'NONE', #16067, #18091 ) ;
#14526 = LINE ( 'NONE', #5586, #3448 ) ;
#14527 = PLANE ( 'NONE',  #10993 ) ;
#14528 = CARTESIAN_POINT ( 'NONE',  ( 32.50000000000000000, 40.03620104880000241, -143.0552959529999839 ) ) ;
#14529 = CARTESIAN_POINT ( 'NONE',  ( 3.999999999879999546, -2.250000000000000000, -135.4552959529999896 ) ) ;
#14530 = VECTOR ( 'NONE', #16160, 1000.000000000000000 ) ;
#14531 = ORIENTED_EDGE ( 'NONE', *, *, #6259, .F. ) ;
#14532 = AXIS2_PLACEMENT_3D ( 'NONE', #1256, #17296, #19196 ) ;
#14533 = AXIS2_PLACEMENT_3D ( 'NONE', #8097, #12994, #20724 ) ;
#14534 = DIRECTION ( 'NONE',  ( 0.000000000000000000, 1.000000000000000000, 0.000000000000000000 ) ) ;
#14535 = FACE_OUTER_BOUND ( 'NONE', #17952, .T. ) ;
#14536 = CARTESIAN_POINT ( 'NONE',  ( -34.35824191590000254, -18.00000000000000000, -141.0657682190000060 ) ) ;
#14537 = CARTESIAN_POINT ( 'NONE',  ( -4.929500267440261041, 40.76073806058817439, -141.9202204794446232 ) ) ;
#14538 = DIRECTION ( 'NONE',  ( 0.000000000000000000, 0.000000000000000000, 1.000000000000000000 ) ) ;
#14539 = VERTEX_POINT ( 'NONE', #4257 ) ;
#14540 = CARTESIAN_POINT ( 'NONE',  ( -26.86882954950000268, 40.29793777999999804, -142.0811670120000088 ) ) ;
#14541 = CARTESIAN_POINT ( 'NONE',  ( -13.86630785140000022, -51.00000000000000000, -136.0552959530000123 ) ) ;
#14542 = ORIENTED_EDGE ( 'NONE', *, *, #1588, .F. ) ;
#14543 = PRESENTATION_LAYER_ASSIGNMENT (  '', '', ( #9202 ) ) ;
#14544 = CARTESIAN_POINT ( 'NONE',  ( -6.049191701419999845, -14.51144913589999952, -145.5552959529999839 ) ) ;
#14545 = EDGE_LOOP ( 'NONE', ( #20316, #2005, #436, #1201, #21257 ) ) ;
#14546 = VECTOR ( 'NONE', #17714, 999.9999999999998863 ) ;
#14547 = DIRECTION ( 'NONE',  ( 0.000000000000000000, -1.000000000000000000, 0.000000000000000000 ) ) ;
#14548 = EDGE_CURVE ( 'NONE', #10902, #9077, #16864, .T. ) ;
#14549 = LINE ( 'NONE', #5606, #246 ) ;
#14550 = CARTESIAN_POINT ( 'NONE',  ( -3.499999999949999996, 42.50000000000000000, -150.0552959529999839 ) ) ;
#14551 = CARTESIAN_POINT ( 'NONE',  ( 7.000004459280741109, 37.19153793952586540, -141.5553035005532649 ) ) ;
#14552 = ORIENTED_EDGE ( 'NONE', *, *, #21704, .T. ) ;
#14553 = CARTESIAN_POINT ( 'NONE',  ( -11.06913245161039860, 35.13609156430476332, -139.6650812237304820 ) ) ;
#14554 = CARTESIAN_POINT ( 'NONE',  ( -19.91220883949999987, 32.96944242089999477, -141.9853941000000077 ) ) ;
#14555 = CARTESIAN_POINT ( 'NONE',  ( -2.121568318600000058, -15.32705806070000243, -143.5552959529999839 ) ) ;
#14556 = CARTESIAN_POINT ( 'NONE',  ( 6.446555752746835566, -30.75005219093839415, -136.0552959530145642 ) ) ;
#14557 = VERTEX_POINT ( 'NONE', #2246 ) ;
#14558 = DIRECTION ( 'NONE',  ( 1.000000000000000000, 0.000000000000000000, 0.000000000000000000 ) ) ;
#14559 =( NAMED_UNIT ( * ) PLANE_ANGLE_UNIT ( ) SI_UNIT ( $, .RADIAN. ) );
#14560 = EDGE_LOOP ( 'NONE', ( #1040, #15937, #21575, #16685, #17175 ) ) ;
#14561 = FACE_OUTER_BOUND ( 'NONE', #11911, .T. ) ;
#14562 = PLANE ( 'NONE',  #14131 ) ;
#14563 = PLANE ( 'NONE',  #7746 ) ;
#14564 = EDGE_LOOP ( 'NONE', ( #7939, #21400, #11244, #19678 ) ) ;
#14565 = CARTESIAN_POINT ( 'NONE',  ( 13.68320006080000084, -21.50000000000000000, -148.5552959529999839 ) ) ;
#14566 = DIRECTION ( 'NONE',  ( -1.000000000000000000, 0.000000000000000000, 0.000000000000000000 ) ) ;
#14567 = ORIENTED_EDGE ( 'NONE', *, *, #12655, .T. ) ;
#14568 = LINE ( 'NONE', #14211, #22829 ) ;
#14569 = CARTESIAN_POINT ( 'NONE',  ( 16.87269471589999981, -31.91616505980000085, -143.5552959529999839 ) ) ;
#14570 = CARTESIAN_POINT ( 'NONE',  ( -15.91988638306137815, -44.20085980601010789, -150.0552959529999839 ) ) ;
#14571 = CARTESIAN_POINT ( 'NONE',  ( 3.611688725869999975E-11, 47.50000000000000000, -136.0552959530000123 ) ) ;
#14572 = EDGE_CURVE ( 'NONE', #20428, #14060, #18769, .T. ) ;
#14573 = DIRECTION ( 'NONE',  ( 2.255973186040000320E-12, 0.000000000000000000, 1.000000000000000000 ) ) ;
#14574 = CARTESIAN_POINT ( 'NONE',  ( 15.10199673422965816, 39.50000000000000000, -150.0552959529999839 ) ) ;
#14575 = ITEM_DEFINED_TRANSFORMATION ( 'NONE', 'NONE', #10746,  #5025 ) ;
#14576 = DIRECTION ( 'NONE',  ( -0.000000000000000000, 1.000000000000000000, 0.000000000000000000 ) ) ;
#14577 = EDGE_CURVE ( 'NONE', #16847, #19447, #7465, .T. ) ;
#14578 = PLANE ( 'NONE',  #8930 ) ;
#14579 = DIRECTION ( 'NONE',  ( 1.526468026909999897E-13, 8.159623473500000156E-13, 1.000000000000000000 ) ) ;
#14580 = ORIENTED_EDGE ( 'NONE', *, *, #1503, .F. ) ;
#14581 = VERTEX_POINT ( 'NONE', #9471 ) ;
#14582 = ORIENTED_EDGE ( 'NONE', *, *, #1484, .F. ) ;
#14583 = CARTESIAN_POINT ( 'NONE',  ( -16.71251657190000017, 33.01037093000000766, -141.5651630139999781 ) ) ;
#14584 = FACE_OUTER_BOUND ( 'NONE', #10689, .T. ) ;
#14585 = DIRECTION ( 'NONE',  ( 0.000000000000000000, 1.000000000000000000, 0.000000000000000000 ) ) ;
#14586 = LINE ( 'NONE', #3526, #20286 ) ;
#14587 = EDGE_LOOP ( 'NONE', ( #18866, #6021, #17772, #17060 ) ) ;
#14588 = CARTESIAN_POINT ( 'NONE',  ( -4.881030538584610667, 24.01480899504991484, -150.0552959529999839 ) ) ;
#14589 = CARTESIAN_POINT ( 'NONE',  ( -19.15756699511638317, 33.51755048520087854, -143.8372150283107374 ) ) ;
#14590 = DIRECTION ( 'NONE',  ( -0.1000233216789610108, -0.9949850929136109245, 3.600083194518594546E-13 ) ) ;
#14591 = VERTEX_POINT ( 'NONE', #5802 ) ;
#14592 = DIRECTION ( 'NONE',  ( -1.527666881879999979E-13, -8.171241461240000022E-13, -1.000000000000000000 ) ) ;
#14593 = ADVANCED_FACE ( 'NONE', ( #20441 ), #11010, .F. ) ;
#14594 = ORIENTED_EDGE ( 'NONE', *, *, #18120, .F. ) ;
#14595 = CARTESIAN_POINT ( 'NONE',  ( 8.774234277345202671, 35.52522618527662956, -142.0366557234719380 ) ) ;
#14596 = LINE ( 'NONE', #13038, #11974 ) ;
#14597 = PLANE ( 'NONE',  #6441 ) ;
#14598 = EDGE_CURVE ( 'NONE', #11995, #23456, #19119, .T. ) ;
#14599 = VERTEX_POINT ( 'NONE', #15427 ) ;
#14600 = CARTESIAN_POINT ( 'NONE',  ( -35.47299999999999898, 14.00000000000000000, -144.0552959529999839 ) ) ;
#14601 = ORIENTED_EDGE ( 'NONE', *, *, #1263, .F. ) ;
#14602 = FILL_AREA_STYLE ('',( #21977 ) ) ;
#14603 = LINE ( 'NONE', #5556, #6698 ) ;
#14604 = VERTEX_POINT ( 'NONE', #22817 ) ;
#14605 = EDGE_LOOP ( 'NONE', ( #22474, #297 ) ) ;
#14606 = VECTOR ( 'NONE', #20406, 1000.000000000000000 ) ;
#14607 = FACE_OUTER_BOUND ( 'NONE', #8419, .T. ) ;
#14608 = EDGE_CURVE ( 'NONE', #3481, #21363, #18969, .T. ) ;
#14609 = CARTESIAN_POINT ( 'NONE',  ( -21.35824191589999899, -31.25000000000000000, -145.5657682190000060 ) ) ;
#14610 = ORIENTED_EDGE ( 'NONE', *, *, #15638, .F. ) ;
#14611 = DIRECTION ( 'NONE',  ( 2.257144641397276061E-12, 2.720901168964863311E-24, 1.000000000000000000 ) ) ;
#14612 = PRODUCT_DEFINITION_SHAPE ( 'NONE', 'NONE',  #6720 ) ;
#14613 = ORIENTED_EDGE ( 'NONE', *, *, #6255, .F. ) ;
#14614 = CARTESIAN_POINT ( 'NONE',  ( 3.611688725869999975E-11, -50.50000000000000000, -136.0552959530000123 ) ) ;
#14615 = DIRECTION ( 'NONE',  ( 2.257749542879999954E-12, 0.000000000000000000, 1.000000000000000000 ) ) ;
#14616 = DIRECTION ( 'NONE',  ( 0.000000000000000000, -1.000000000000000000, 0.000000000000000000 ) ) ;
#14617 = PLANE ( 'NONE',  #14848 ) ;
#14618 = EDGE_CURVE ( 'NONE', #15247, #4592, #20920, .T. ) ;
#14619 = FACE_OUTER_BOUND ( 'NONE', #10359, .T. ) ;
#14620 = EDGE_LOOP ( 'NONE', ( #22219, #734, #19627, #2771 ) ) ;
#14621 = EDGE_CURVE ( 'NONE', #11240, #11694, #2824, .T. ) ;
#14622 = CARTESIAN_POINT ( 'NONE',  ( -13.38748872360000064, 33.38537881989999789, -144.5933708990000071 ) ) ;
#14623 = EDGE_CURVE ( 'NONE', #8854, #13529, #21034, .T. ) ;
#14624 = CARTESIAN_POINT ( 'NONE',  ( 13.13369214859999978, 50.99999999970000175, -136.0552959530000123 ) ) ;
#14625 = ADVANCED_FACE ( 'NONE', ( #4841 ), #7881, .F. ) ;
#14626 = VERTEX_POINT ( 'NONE', #8002 ) ;
#14627 = DIRECTION ( 'NONE',  ( -2.507771768020000122E-12, 0.000000000000000000, 1.000000000000000000 ) ) ;
#14628 = LINE ( 'NONE', #21663, #5519 ) ;
#14629 = CARTESIAN_POINT ( 'NONE',  ( -16.44879669585063908, 37.92811585471407199, -139.9493606072290390 ) ) ;
#14630 = CARTESIAN_POINT ( 'NONE',  ( -22.82643395159999855, 32.86988923359999859, -143.6006525860000238 ) ) ;
#14631 = ORIENTED_EDGE ( 'NONE', *, *, #17675, .T. ) ;
#14632 = CARTESIAN_POINT ( 'NONE',  ( 18.95053822279999878, -50.00000000000000000, -151.0552959529999839 ) ) ;
#14633 = CARTESIAN_POINT ( 'NONE',  ( 6.499999999879999102, -3.500000000000000000, -135.0552959530000123 ) ) ;
#14634 = DIRECTION ( 'NONE',  ( -2.423380700840000070E-27, 0.000000000000000000, -1.000000000000000000 ) ) ;
#14635 = CARTESIAN_POINT ( 'NONE',  ( 12.50000000020000002, 20.50000000000000000, -139.5552959529999839 ) ) ;
#14636 = FACE_OUTER_BOUND ( 'NONE', #13406, .T. ) ;
#14637 = CARTESIAN_POINT ( 'NONE',  ( -31.00000000000000000, 1.000000000000000000, -149.5552959529999839 ) ) ;
#14638 = ORIENTED_EDGE ( 'NONE', *, *, #20595, .T. ) ;
#14639 = EDGE_CURVE ( 'NONE', #968, #20332, #2205, .T. ) ;
#14640 =( BOUNDED_SURFACE ( )  B_SPLINE_SURFACE ( 5, 5, ( 
 ( #12919, #2107, #9329, #14832, #15654, #17310 ),
 ( #1152, #15526, #19335, #10284, #2572, #18980 ),
 ( #12064, #22791, #911, #21011, #8253, #11701 ),
 ( #8135, #15407, #6131, #3047, #6489, #15301 ),
 ( #1025, #4703, #13495, #22914, #22666, #20654 ),
 ( #6598, #2922, #17072, #9919, #20770, #1272 ),
 ( #6362, #11943, #17556, #13747, #15178, #9794 ),
 ( #13386, #4464, #794, #22436, #2804, #10034 ),
 ( #8385, #20895, #19211, #4349, #11583, #2692 ),
 ( #13862, #17426, #17192, #13618, #10154, #4584 ),
 ( #21129, #4822, #11824, #18861, #8017, #22557 ),
 ( #6246, #19099, #16122, #12533, #14218, #7073 ) ),
 .UNSPECIFIED., .F., .F., .F. ) 
 B_SPLINE_SURFACE_WITH_KNOTS ( ( 6, 3, 3, 6 ),
 ( 6, 6 ),
 ( 0.000000000000000000, 4.454241660750000165, 8.943513424000000711, 13.47090878500000066 ),
 ( 1.570796326706449975, 3.141592653590000062 ),
 .UNSPECIFIED. ) 
 GEOMETRIC_REPRESENTATION_ITEM ( )  RATIONAL_B_SPLINE_SURFACE ( (
 ( 0.2500000000000000000, 0.2499999999887249913, 0.2999999999830880171, 0.3999999999774505044, 0.5999999999774500159, 1.000000000000000000),
 ( 0.2500000000000000000, 0.2499999999887249913, 0.2999999999830880171, 0.3999999999774505044, 0.5999999999774500159, 1.000000000000000000),
 ( 0.2500000000000000000, 0.2499999999887249913, 0.2999999999830880171, 0.3999999999774505044, 0.5999999999774500159, 1.000000000000000000),
 ( 0.2500000000000000000, 0.2499999999887249913, 0.2999999999830880171, 0.3999999999774505044, 0.5999999999774500159, 1.000000000000000000),
 ( 0.2500000000000000000, 0.2499999999887249913, 0.2999999999830880171, 0.3999999999774505044, 0.5999999999774500159, 1.000000000000000000),
 ( 0.2500000000000000000, 0.2499999999887249913, 0.2999999999830880171, 0.3999999999774505044, 0.5999999999774500159, 1.000000000000000000),
 ( 0.2500000000000000000, 0.2499999999887249913, 0.2999999999830880171, 0.3999999999774505044, 0.5999999999774500159, 1.000000000000000000),
 ( 0.2500000000000000000, 0.2499999999887249913, 0.2999999999830880171, 0.3999999999774505044, 0.5999999999774500159, 1.000000000000000000),
 ( 0.2500000000000000000, 0.2499999999887249913, 0.2999999999830880171, 0.3999999999774505044, 0.5999999999774500159, 1.000000000000000000),
 ( 0.2500000000000000000, 0.2499999999887249913, 0.2999999999830880171, 0.3999999999774505044, 0.5999999999774500159, 1.000000000000000000),
 ( 0.2500000000000000000, 0.2499999999887249913, 0.2999999999830880171, 0.3999999999774505044, 0.5999999999774500159, 1.000000000000000000),
 ( 0.2500000000000000000, 0.2499999999887249913, 0.2999999999830880171, 0.3999999999774505044, 0.5999999999774500159, 1.000000000000000000) ) ) 
 REPRESENTATION_ITEM ( '' )  SURFACE ( )  );
#14641 = FILL_AREA_STYLE_COLOUR ( '', #14116 ) ;
#14642 = CARTESIAN_POINT ( 'NONE',  ( -4.500000000000000000, 40.00000000000000000, -150.0552959529999839 ) ) ;
#14643 = FACE_OUTER_BOUND ( 'NONE', #2427, .T. ) ;
#14644 = CARTESIAN_POINT ( 'NONE',  ( -4.818372690434668648, 39.73127005685628177, -140.3607218662884009 ) ) ;
#14645 = DIRECTION ( 'NONE',  ( 0.000000000000000000, 1.000000000000000000, 0.000000000000000000 ) ) ;
#14646 = ORIENTED_EDGE ( 'NONE', *, *, #393, .F. ) ;
#14647 = EDGE_CURVE ( 'NONE', #4899, #18413, #14424, .T. ) ;
#14648 = DIRECTION ( 'NONE',  ( 0.1000233216789610108, 0.9949850929136109245, -3.588240815588595806E-13 ) ) ;
#14649 = EDGE_CURVE ( 'NONE', #4401, #20657, #18489, .T. ) ;
#14650 = CARTESIAN_POINT ( 'NONE',  ( -9.923478264230000789, -23.29931827799999766, -143.5552959529999839 ) ) ;
#14651 = VERTEX_POINT ( 'NONE', #13367 ) ;
#14652 = ORIENTED_EDGE ( 'NONE', *, *, #1406, .T. ) ;
#14653 = CARTESIAN_POINT ( 'NONE',  ( 4.698860268592982337, -1.999999999999998224, -136.0552959530106421 ) ) ;
#14654 = LINE ( 'NONE', #7394, #18093 ) ;
#14655 = CARTESIAN_POINT ( 'NONE',  ( -22.03156944979999921, 33.39557638549999297, -141.8445571070000142 ) ) ;
#14656 = FACE_OUTER_BOUND ( 'NONE', #19160, .T. ) ;
#14657 = VECTOR ( 'NONE', #1126, 1000.000000000000000 ) ;
#14658 = ORIENTED_EDGE ( 'NONE', *, *, #22090, .F. ) ;
#14659 = CARTESIAN_POINT ( 'NONE',  ( -11.37294983628254208, 34.64303755342024971, -140.7164989729878641 ) ) ;
#14660 = VECTOR ( 'NONE', #5777, 1000.000000000000000 ) ;
#14661 = CARTESIAN_POINT ( 'NONE',  ( -18.80491877122047129, 35.17450263849315917, -148.4239332058163825 ) ) ;
#14662 = LINE ( 'NONE', #22045, #5628 ) ;
#14663 = CYLINDRICAL_SURFACE ( 'NONE', #18315, 0.5000000000000004441 ) ;
#14664 = CARTESIAN_POINT ( 'NONE',  ( 22.36721601470000209, -21.34320095609999868, -147.5552959529999839 ) ) ;
#14665 = CARTESIAN_POINT ( 'NONE',  ( 25.31684607440000079, 45.26810052429999587, -149.5552959529999839 ) ) ;
#14666 = CARTESIAN_POINT ( 'NONE',  ( 19.16617820230000291, 49.81753540199999719, -149.5552959529999839 ) ) ;
#14667 = PLANE ( 'NONE',  #5012 ) ;
#14668 = CARTESIAN_POINT ( 'NONE',  ( 12.91075631260000023, -38.04527125359999928, -147.5552959529999839 ) ) ;
#14669 = VERTEX_POINT ( 'NONE', #22538 ) ;
#14670 = ADVANCED_FACE ( 'NONE', ( #9775, #18958 ), #418, .T. ) ;
#14671 = CARTESIAN_POINT ( 'NONE',  ( -6.289131962756090211, 37.69042679468366686, -147.3987319627627812 ) ) ;
#14672 = EDGE_CURVE ( 'NONE', #22590, #4093, #2329, .T. ) ;
#14673 = AXIS2_PLACEMENT_3D ( 'NONE', #10224, #17496, #22975 ) ;
#14674 = AXIS2_PLACEMENT_3D ( 'NONE', #11673, #22530, #6334 ) ;
#14675 = ORIENTED_EDGE ( 'NONE', *, *, #9948, .F. ) ;
#14676 =( NAMED_UNIT ( * ) SI_UNIT ( $, .STERADIAN. ) SOLID_ANGLE_UNIT ( ) );
#14677 = DIRECTION ( 'NONE',  ( 0.000000000000000000, 7.159923868353169372E-11, -1.000000000000000000 ) ) ;
#14678 = CARTESIAN_POINT ( 'NONE',  ( 20.58976242830000203, -31.80400447969999789, -142.5552959529999839 ) ) ;
#14679 = DIRECTION ( 'NONE',  ( -1.211690350419999855E-27, -2.765629237169980113E-27, 1.000000000000000000 ) ) ;
#14680 = DIRECTION ( 'NONE',  ( -1.527666881879999979E-13, -8.171241461240000022E-13, -1.000000000000000000 ) ) ;
#14681 = DIRECTION ( 'NONE',  ( 1.000000000000000000, 0.000000000000000000, -4.510774274160000731E-12 ) ) ;
#14682 = DIRECTION ( 'NONE',  ( -0.1000233216789610108, -0.9949850929136109245, 3.600083194518594546E-13 ) ) ;
#14683 = CARTESIAN_POINT ( 'NONE',  ( -3.500000000000000000, 42.50000000000000000, -151.0552959529999839 ) ) ;
#14684 = CARTESIAN_POINT ( 'NONE',  ( -32.50000000000000000, -43.00000000050000182, -137.0552959530000123 ) ) ;
#14685 = ORIENTED_EDGE ( 'NONE', *, *, #15873, .F. ) ;
#14686 = VECTOR ( 'NONE', #19156, 1000.000000000000000 ) ;
#14687 = PRODUCT_DEFINITION_CONTEXT ( 'detailed design', #21353, 'design' ) ;
#14688 = ORIENTED_EDGE ( 'NONE', *, *, #3995, .T. ) ;
#14689 = ORIENTED_EDGE ( 'NONE', *, *, #13885, .F. ) ;
#14690 = DIRECTION ( 'NONE',  ( 4.430318231636154847E-12, -6.100259101445539707E-13, 1.000000000000000000 ) ) ;
#14691 = CARTESIAN_POINT ( 'NONE',  ( -9.394779979509999990, -17.86685386420000299, -143.5552959529999839 ) ) ;
#14692 = CARTESIAN_POINT ( 'NONE',  ( -31.50000000000000000, -36.00000000000000000, -143.3052959529999839 ) ) ;
#14693 = EDGE_LOOP ( 'NONE', ( #12100, #20577, #14255, #3461 ) ) ;
#14694 = EDGE_CURVE ( 'NONE', #15850, #2337, #6805, .T. ) ;
#14695 = CARTESIAN_POINT ( 'NONE',  ( 1.829659965300000080, -16.02499107890000118, -144.5552959529999839 ) ) ;
#14696 = CARTESIAN_POINT ( 'NONE',  ( -18.64600821060120239, 33.72696025750419579, -146.0724859999907892 ) ) ;
#14697 = ADVANCED_FACE ( 'NONE', ( #18736 ), #16507, .F. ) ;
#14698 = CARTESIAN_POINT ( 'NONE',  ( 32.00000000000000000, -21.03620104879999886, -137.0552959530000123 ) ) ;
#14699 = EDGE_LOOP ( 'NONE', ( #1777, #8643, #14003, #9577 ) ) ;
#14700 = CARTESIAN_POINT ( 'NONE',  ( 8.931951867280000457, -17.52729875919999714, -143.0552959529999839 ) ) ;
#14701 = AXIS2_PLACEMENT_3D ( 'NONE', #2665, #15384, #999 ) ;
#14702 = CARTESIAN_POINT ( 'NONE',  ( 6.000000000050000004, 37.00000000000000000, -148.0552959529999839 ) ) ;
#14703 = AXIS2_PLACEMENT_3D ( 'NONE', #14518, #3101, #4997 ) ;
#14704 = LINE ( 'NONE', #3891, #8557 ) ;
#14705 = FACE_BOUND ( 'NONE', #18744, .T. ) ;
#14706 = ORIENTED_EDGE ( 'NONE', *, *, #13018, .T. ) ;
#14707 = CARTESIAN_POINT ( 'NONE',  ( -32.50000000000000000, 28.00000000000000000, -144.0552959529999839 ) ) ;
#14708 = ORIENTED_EDGE ( 'NONE', *, *, #354, .T. ) ;
#14709 = CARTESIAN_POINT ( 'NONE',  ( 31.00000000000000000, -39.80430157320000006, -150.5552959529999839 ) ) ;
#14711 = ORIENTED_EDGE ( 'NONE', *, *, #11668, .T. ) ;
#14710 = VECTOR ( 'NONE', #13782, 1000.000000000000227 ) ;
#14712 = CARTESIAN_POINT ( 'NONE',  ( -26.11027262183172226, 40.79568045835033274, -143.6926091179167315 ) ) ;
#14713 = ORIENTED_EDGE ( 'NONE', *, *, #20439, .F. ) ;
#14714 = LINE ( 'NONE', #21982, #17451 ) ;
#14715 = AXIS2_PLACEMENT_3D ( 'NONE', #735, #7972, #13097 ) ;
#14716 = EDGE_LOOP ( 'NONE', ( #17348, #16779, #21053, #15692 ) ) ;
#14717 = DIRECTION ( 'NONE',  ( -0.000000000000000000, 1.000000000000000000, 0.000000000000000000 ) ) ;
#14718 = ORIENTED_EDGE ( 'NONE', *, *, #13125, .T. ) ;
#14719 = CIRCLE ( 'NONE', #13959, 5.000000000000000888 ) ;
#14720 = ORIENTED_EDGE ( 'NONE', *, *, #11423, .F. ) ;
#14721 = CARTESIAN_POINT ( 'NONE',  ( -35.73252798949999942, 47.50000000000000000, -138.5552959529999839 ) ) ;
#14722 = CARTESIAN_POINT ( 'NONE',  ( -32.50000000000000000, 21.50000000000000000, -151.0552959529999839 ) ) ;
#14723 = CARTESIAN_POINT ( 'NONE',  ( 7.480639893028359744, 27.95196862336024779, -150.0552959529999839 ) ) ;
#14724 = EDGE_CURVE ( 'NONE', #14338, #20751, #19301, .T. ) ;
#14725 = CARTESIAN_POINT ( 'NONE',  ( 7.683200060759999950, -20.50000000000000000, -148.5552959529999839 ) ) ;
#14726 = CARTESIAN_POINT ( 'NONE',  ( -10.42144917147403227, 35.06776031302221952, -141.1445986588747132 ) ) ;
#14727 = CARTESIAN_POINT ( 'NONE',  ( -7.880169906864895601, 39.70507027285627544, -140.3906468505855685 ) ) ;
#14728 = ORIENTED_EDGE ( 'NONE', *, *, #4417, .F. ) ;
#14729 = DIRECTION ( 'NONE',  ( 0.000000000000000000, -2.256894259950000208E-12, 1.000000000000000000 ) ) ;
#14731 = VECTOR ( 'NONE', #13692, 1000.000000000000000 ) ;
#14730 = PRODUCT_RELATED_PRODUCT_CATEGORY ( 'part', '', ( #19655 ) ) ;
#14732 = DIRECTION ( 'NONE',  ( 1.000000000000000000, 0.000000000000000000, 0.000000000000000000 ) ) ;
#14733 = EDGE_CURVE ( 'NONE', #19891, #7656, #6569, .T. ) ;
#14734 = COLOUR_RGB ( '', 0.72549020, 0.75294118, 0.79215686) ;
#14735 = ORIENTED_EDGE ( 'NONE', *, *, #15241, .T. ) ;
#14736 = DIRECTION ( 'NONE',  ( 0.9944529286486341046, -0.1051825684329612265, -4.470295960598355531E-12 ) ) ;
#14737 = CYLINDRICAL_SURFACE ( 'NONE', #3623, 0.5000000000000079936 ) ;
#14738 = CARTESIAN_POINT ( 'NONE',  ( -17.81604679228244237, 41.73690735279433994, -144.4734149966611199 ) ) ;
#14739 = CARTESIAN_POINT ( 'NONE',  ( -29.15022769660199131, 39.64481412623220535, -141.5404043871726287 ) ) ;
#14740 = ORIENTED_EDGE ( 'NONE', *, *, #3588, .F. ) ;
#14741 = CARTESIAN_POINT ( 'NONE',  ( -12.50000000000000000, 25.50000000000000000, -137.0552959530000123 ) ) ;
#14742 = DIRECTION ( 'NONE',  ( 2.257305453670000045E-12, 0.000000000000000000, 1.000000000000000000 ) ) ;
#14743 = EDGE_CURVE ( 'NONE', #13536, #13650, #2891, .T. ) ;
#14744 = CARTESIAN_POINT ( 'NONE',  ( 23.21181482502168336, -23.48612613680713679, -144.7152959529975362 ) ) ;
#14745 = CARTESIAN_POINT ( 'NONE',  ( 6.500000000159999125, 20.50000000000000000, -140.5552959529999839 ) ) ;
#14746 = DIRECTION ( 'NONE',  ( -1.000000000000000000, 0.000000000000000000, -1.211690350419999855E-27 ) ) ;
#14747 = CARTESIAN_POINT ( 'NONE',  ( -5.499999999999999112, 44.76520911280726267, -150.0552959530000123 ) ) ;
#14748 = CARTESIAN_POINT ( 'NONE',  ( -19.75449977488149855, 38.96382659270718563, -139.8356432587078189 ) ) ;
#14749 = VERTEX_POINT ( 'NONE', #10005 ) ;
#14750 = CARTESIAN_POINT ( 'NONE',  ( -27.87941100700000163, 36.27261185799999765, -147.6334388379999893 ) ) ;
#14751 = EDGE_CURVE ( 'NONE', #15247, #18803, #5295, .T. ) ;
#14752 = VECTOR ( 'NONE', #5758, 1000.000000000000227 ) ;
#14753 = LINE ( 'NONE', #12965, #3068 ) ;
#14754 = DIRECTION ( 'NONE',  ( 1.526468026909680062E-13, 8.159623473499330697E-13, 1.000000000000000000 ) ) ;
#14755 = CIRCLE ( 'NONE', #14386, 9.999999999999998224 ) ;
#14756 = LINE ( 'NONE', #16891, #2393 ) ;
#14757 = LINE ( 'NONE', #2282, #3415 ) ;
#14758 = VERTEX_POINT ( 'NONE', #8223 ) ;
#14759 = CARTESIAN_POINT ( 'NONE',  ( -30.49999999990000177, 29.00000000000000000, -147.5552959529999839 ) ) ;
#14760 = CARTESIAN_POINT ( 'NONE',  ( -16.16658683009994490, 37.07694188521399070, -148.2333767341115447 ) ) ;
#14761 = EDGE_LOOP ( 'NONE', ( #10906, #5447, #6905, #19426 ) ) ;
#14762 = ADVANCED_FACE ( 'NONE', ( #15492 ), #10122, .F. ) ;
#14763 = EDGE_CURVE ( 'NONE', #10310, #14581, #13710, .T. ) ;
#14764 = ORIENTED_EDGE ( 'NONE', *, *, #2565, .F. ) ;
#14765 = ADVANCED_FACE ( 'NONE', ( #19543 ), #12032, .F. ) ;
#14766 = CARTESIAN_POINT ( 'NONE',  ( -32.50000000000000000, 47.50000000000000000, -151.0552959529999839 ) ) ;
#14767 = AXIS2_PLACEMENT_3D ( 'NONE', #16202, #1589, #5716 ) ;
#14768 = VECTOR ( 'NONE', #2024, 1000.000000000000000 ) ;
#14769 = CARTESIAN_POINT ( 'NONE',  ( -24.06602356359999817, 36.94557182220000158, -148.2530914610000252 ) ) ;
#14770 = CIRCLE ( 'NONE', #17038, 1.500000000000001332 ) ;
#14771 = CARTESIAN_POINT ( 'NONE',  ( -3.499999999949999996, 34.00000000000000000, -150.0552959529999839 ) ) ;
#14772 = LINE ( 'NONE', #12982, #15941 ) ;
#14773 = VERTEX_POINT ( 'NONE', #14858 ) ;
#14774 = CARTESIAN_POINT ( 'NONE',  ( -5.316799939240000938, 3.500000000000000000, -148.5552959529999839 ) ) ;
#14775 = CARTESIAN_POINT ( 'NONE',  ( -19.09494877088048170, 33.54410563151299840, -142.1858765933287998 ) ) ;
#14776 = VECTOR ( 'NONE', #12228, 1000.000000000000000 ) ;
#14777 = EDGE_CURVE ( 'NONE', #4867, #10143, #18598, .T. ) ;
#14778 = DIRECTION ( 'NONE',  ( 1.000000000000000000, 0.000000000000000000, 0.000000000000000000 ) ) ;
#14779 = CARTESIAN_POINT ( 'NONE',  ( 13.66060904168811696, 34.09818317340324256, -136.0552959530308783 ) ) ;
#14780 = AXIS2_PLACEMENT_3D ( 'NONE', #4172, #2285, #18798 ) ;
#14781 = CARTESIAN_POINT ( 'NONE',  ( -24.60556451751816454, 40.79665324755396227, -146.2317373473354394 ) ) ;
#14782 = ADVANCED_FACE ( 'NONE', ( #7586 ), #20225, .F. ) ;
#14783 = CARTESIAN_POINT ( 'NONE',  ( -15.03800142071511914, 35.98415342847451370, -148.3589868715107229 ) ) ;
#14784 = EDGE_CURVE ( 'NONE', #21963, #14843, #13265, .T. ) ;
#14785 = ADVANCED_FACE ( 'NONE', ( #12945 ), #14968, .F. ) ;
#14786 = CARTESIAN_POINT ( 'NONE',  ( -7.695630400395947923, 37.03895750127035313, -140.6427397355593030 ) ) ;
#14787 = LINE ( 'NONE', #16682, #6137 ) ;
#14788 = DIRECTION ( 'NONE',  ( 0.000000000000000000, 0.000000000000000000, 1.000000000000000000 ) ) ;
#14789 = VECTOR ( 'NONE', #20676, 999.9999999999998863 ) ;
#14790 = ORIENTED_EDGE ( 'NONE', *, *, #17932, .T. ) ;
#14791 = CARTESIAN_POINT ( 'NONE',  ( -5.543976733014329028, 40.02318592805595188, -142.2744635965945008 ) ) ;
#14792 = B_SPLINE_CURVE_WITH_KNOTS ( 'NONE', 1,
 ( #188, #17181 ),
 .UNSPECIFIED., .F., .F.,
 ( 2, 2 ),
 ( -15.50174796760000007, 0.2824781943659999683 ),
 .UNSPECIFIED. ) ;
#14793 = VECTOR ( 'NONE', #16091, 1000.000000000000000 ) ;
#14794 = VERTEX_POINT ( 'NONE', #578 ) ;
#14795 = CARTESIAN_POINT ( 'NONE',  ( 17.21087225569999646, -22.66053313549999970, -145.5552959529999839 ) ) ;
#14796 = VECTOR ( 'NONE', #12231, 1000.000000000000114 ) ;
#14797 = VECTOR ( 'NONE', #9596, 1000.000000000000000 ) ;
#14798 = DIRECTION ( 'NONE',  ( -2.257144641399999941E-12, 0.000000000000000000, -1.000000000000000000 ) ) ;
#14799 = CARTESIAN_POINT ( 'NONE',  ( 2.170391987449999505, -12.72823260819999902, -146.5552959529999839 ) ) ;
#14800 = CYLINDRICAL_SURFACE ( 'NONE', #22755, 2.000000000000001776 ) ;
#14801 = ORIENTED_EDGE ( 'NONE', *, *, #4844, .F. ) ;
#14802 = CARTESIAN_POINT ( 'NONE',  ( -13.82353779674532035, 34.78290842721720111, -141.1681162278709962 ) ) ;
#14803 = CARTESIAN_POINT ( 'NONE',  ( 6.000000000140000012, 36.50000000000000000, -147.0552959529999839 ) ) ;
#14804 = CARTESIAN_POINT ( 'NONE',  ( 19.27350934360000068, 50.38169314270000143, -143.0552959529999839 ) ) ;
#14805 = FACE_OUTER_BOUND ( 'NONE', #11444, .T. ) ;
#14806 = CARTESIAN_POINT ( 'NONE',  ( 0.000000000000000000, 34.00000000000000000, -150.0552959529999839 ) ) ;
#14807 = VECTOR ( 'NONE', #17397, 1000.000000000000000 ) ;
#14808 = DIRECTION ( 'NONE',  ( 0.000000000000000000, 1.000000000000000000, 0.000000000000000000 ) ) ;
#14809 = APPLICATION_CONTEXT ( 'automotive_design' ) ;
#14810 = CIRCLE ( 'NONE', #19755, 0.7500000000000006661 ) ;
#14811 = EDGE_LOOP ( 'NONE', ( #9030, #6221, #9957, #439 ) ) ;
#14812 = EDGE_CURVE ( 'NONE', #4078, #11102, #16414, .T. ) ;
#14813 = VECTOR ( 'NONE', #3908, 1000.000000000000000 ) ;
#14814 = AXIS2_PLACEMENT_3D ( 'NONE', #6376, #17683, #11842 ) ;
#14815 = CARTESIAN_POINT ( 'NONE',  ( -28.35872823665358666, 34.75047554562008401, -147.1914172358262931 ) ) ;
#14816 = VERTEX_POINT ( 'NONE', #123 ) ;
#14817 = VECTOR ( 'NONE', #4382, 1000.000000000000000 ) ;
#14818 = EDGE_LOOP ( 'NONE', ( #6822, #16998, #12459, #6859, #13916, #13869 ) ) ;
#14819 = CARTESIAN_POINT ( 'NONE',  ( -12.76754407576741990, 35.14623324252765002, -148.4212001205290221 ) ) ;
#14820 = CARTESIAN_POINT ( 'NONE',  ( -10.36675979729999852, 34.52853970540000006, -140.3392284379999921 ) ) ;
#14821 = CARTESIAN_POINT ( 'NONE',  ( 8.446000075299080478, 27.76013181716325207, -136.0552959530190549 ) ) ;
#14822 = EDGE_LOOP ( 'NONE', ( #55, #17616 ) ) ;
#14823 = LINE ( 'NONE', #15046, #12538 ) ;
#14824 = CARTESIAN_POINT ( 'NONE',  ( -22.10824191589999899, -32.00000000000000000, -141.0657682190000060 ) ) ;
#14825 = CARTESIAN_POINT ( 'NONE',  ( -31.00000000000000000, -50.00000000000000000, -149.5552959529999839 ) ) ;
#14826 = ORIENTED_EDGE ( 'NONE', *, *, #15525, .T. ) ;
#14827 = CARTESIAN_POINT ( 'NONE',  ( -20.55310894649999653, 37.85259822169999921, -139.7937414779999870 ) ) ;
#14828 = VECTOR ( 'NONE', #8713, 1000.000000000000000 ) ;
#14829 = VECTOR ( 'NONE', #20408, 1000.000000000000000 ) ;
#14830 = LINE ( 'NONE', #22089, #14660 ) ;
#14831 = VECTOR ( 'NONE', #9543, 1000.000000000000227 ) ;
#14832 = CARTESIAN_POINT ( 'NONE',  ( -24.50448663614206168, 36.99790949615556457, -147.3823814620965038 ) ) ;
#14833 = ORIENTED_EDGE ( 'NONE', *, *, #8434, .T. ) ;
#14834 = EDGE_CURVE ( 'NONE', #6817, #23414, #18195, .T. ) ;
#14835 = CARTESIAN_POINT ( 'NONE',  ( -7.499999999969999109, 45.50000000000000000, -137.0552959530000123 ) ) ;
#14836 = ORIENTED_EDGE ( 'NONE', *, *, #15352, .T. ) ;
#14837 = LINE ( 'NONE', #20312, #5630 ) ;
#14838 = EDGE_CURVE ( 'NONE', #15850, #19030, #1912, .T. ) ;
#14839 = VERTEX_POINT ( 'NONE', #5805 ) ;
#14840 = CARTESIAN_POINT ( 'NONE',  ( -26.73151279747740006, 41.02465574082271615, -146.3859699704034085 ) ) ;
#14841 = EDGE_LOOP ( 'NONE', ( #4161, #9907, #3290, #19778 ) ) ;
#14842 = CARTESIAN_POINT ( 'NONE',  ( -22.37814652455998043, 32.77961379161537536, -141.5227465161630107 ) ) ;
#14843 = VERTEX_POINT ( 'NONE', #2252 ) ;
#14844 = CARTESIAN_POINT ( 'NONE',  ( -16.84364015992473540, -45.39900052719455203, -150.0552959529999839 ) ) ;
#14845 = ORIENTED_EDGE ( 'NONE', *, *, #19723, .F. ) ;
#14846 = DIRECTION ( 'NONE',  ( 1.000000000000000000, 0.000000000000000000, 0.000000000000000000 ) ) ;
#14847 = VECTOR ( 'NONE', #6403, 1000.000000000000000 ) ;
#14848 = AXIS2_PLACEMENT_3D ( 'NONE', #3794, #18879, #9700 ) ;
#14849 = ORIENTED_EDGE ( 'NONE', *, *, #3582, .T. ) ;
#14850 = CARTESIAN_POINT ( 'NONE',  ( -27.28682787397352172, 39.84701410126417898, -147.9146130286543439 ) ) ;
#14851 = DIRECTION ( 'NONE',  ( -0.7633862853691523176, 0.6459422414661291079, 1.722923451730345384E-12 ) ) ;
#14852 = CARTESIAN_POINT ( 'NONE',  ( 13.99999999999999822, 20.99298601556613519, -150.0552959529999839 ) ) ;
#14853 = DIRECTION ( 'NONE',  ( 0.000000000000000000, -1.000000000000000000, 3.568879590630000244E-13 ) ) ;
#14854 = CARTESIAN_POINT ( 'NONE',  ( -7.010349701995939320, 37.05829245175783626, -148.1453878980124159 ) ) ;
#14855 = DIRECTION ( 'NONE',  ( 8.956391184260000029E-12, -9.094947017729999296E-13, 1.000000000000000000 ) ) ;
#14856 = ORIENTED_EDGE ( 'NONE', *, *, #980, .T. ) ;
#14857 = LINE ( 'NONE', #22114, #2245 ) ;
#14858 = CARTESIAN_POINT ( 'NONE',  ( 20.50000000000000000, 19.50000000000000000, -150.0552959529999839 ) ) ;
#14859 = AXIS2_PLACEMENT_3D ( 'NONE', #5084, #19724, #12219 ) ;
#14860 = ORIENTED_EDGE ( 'NONE', *, *, #20297, .F. ) ;
#14861 = AXIS2_PLACEMENT_3D ( 'NONE', #20275, #11440, #4079 ) ;
#14862 = DIRECTION ( 'NONE',  ( -1.000000000000000000, 5.094701932209999624E-24, 2.257144641399999941E-12 ) ) ;
#14863 = CARTESIAN_POINT ( 'NONE',  ( -12.13433848750514166, 40.98455321840125976, -141.8124549635463438 ) ) ;
#14864 = EDGE_CURVE ( 'NONE', #18490, #5042, #7364, .T. ) ;
#14865 = CARTESIAN_POINT ( 'NONE',  ( -17.97686571119999854, 41.53571570570000659, -143.4577736070000071 ) ) ;
#14866 = CYLINDRICAL_SURFACE ( 'NONE', #7945, 5.000000000000001776 ) ;
#14867 = ORIENTED_EDGE ( 'NONE', *, *, #10361, .F. ) ;
#14868 = CARTESIAN_POINT ( 'NONE',  ( -6.227860603739999945, 35.34754625490000279, -147.7419925389999946 ) ) ;
#14869 = EDGE_CURVE ( 'NONE', #7407, #14322, #18318, .T. ) ;
#14870 = CARTESIAN_POINT ( 'NONE',  ( 0.000000000000000000, 50.00000000000000000, -150.0552959529999839 ) ) ;
#14871 = ORIENTED_EDGE ( 'NONE', *, *, #21121, .F. ) ;
#14872 = DIRECTION ( 'NONE',  ( 0.000000000000000000, -1.000000000000000000, 0.000000000000000000 ) ) ;
#14873 = CARTESIAN_POINT ( 'NONE',  ( -28.07061429630000049, 34.82490105569999628, -147.0351741510000068 ) ) ;
#14874 = DIRECTION ( 'NONE',  ( 0.000000000000000000, -1.000000000000000000, 0.000000000000000000 ) ) ;
#14875 = CARTESIAN_POINT ( 'NONE',  ( -20.84895621120898923, 41.79397058805413678, -144.6400553131143170 ) ) ;
#14876 = VERTEX_POINT ( 'NONE', #7701 ) ;
#14877 = CARTESIAN_POINT ( 'NONE',  ( -28.42317279839999955, 33.35748734759999934, -144.4144508710000139 ) ) ;
#14878 = DIRECTION ( 'NONE',  ( -0.1000233216789610108, -0.9949850929136109245, 3.591470555298595137E-13 ) ) ;
#14879 = CARTESIAN_POINT ( 'NONE',  ( 25.31684607429999900, -45.26810052439999765, -137.0552959530000123 ) ) ;
#14880 = DIRECTION ( 'NONE',  ( 0.9834926989016489207, 0.1809478134909354718, -4.411697319228424767E-12 ) ) ;
#14881 = CARTESIAN_POINT ( 'NONE',  ( -3.765209112771370492, 42.50000000000001421, -136.0552959529914858 ) ) ;
#14882 = AXIS2_PLACEMENT_3D ( 'NONE', #5482, #10700, #10929 ) ;
#14883 = ORIENTED_EDGE ( 'NONE', *, *, #17842, .F. ) ;
#14884 = DIRECTION ( 'NONE',  ( 0.000000000000000000, 2.256988247090000272E-12, 1.000000000000000000 ) ) ;
#14885 = CARTESIAN_POINT ( 'NONE',  ( -6.683153925719999222, -50.50000000000000000, -136.0552959530000123 ) ) ;
#14886 = ORIENTED_EDGE ( 'NONE', *, *, #8351, .F. ) ;
#14887 = ADVANCED_FACE ( 'NONE', ( #16869 ), #4141, .F. ) ;
#14888 = EDGE_LOOP ( 'NONE', ( #9505, #19371 ) ) ;
#14889 = CYLINDRICAL_SURFACE ( 'NONE', #16957, 8.176568160359995119 ) ;
#14890 = CARTESIAN_POINT ( 'NONE',  ( -31.00000000000000000, -50.00000000000000000, -150.5552959529999839 ) ) ;
#14891 = DIRECTION ( 'NONE',  ( 1.000000000000000000, 0.000000000000000000, -2.259525899719999991E-12 ) ) ;
#14892 = CARTESIAN_POINT ( 'NONE',  ( 7.437582298410791992, 35.94108727011604287, -141.7906281409924816 ) ) ;
#14893 = ORIENTED_EDGE ( 'NONE', *, *, #22784, .T. ) ;
#14894 = CARTESIAN_POINT ( 'NONE',  ( 22.01137100460000084, -15.39610142400000115, -147.0552959529999839 ) ) ;
#14895 = ADVANCED_FACE ( 'NONE', ( #14516 ), #10913, .T. ) ;
#14896 = VECTOR ( 'NONE', #20295, 1000.000000000000000 ) ;
#14897 = CARTESIAN_POINT ( 'NONE',  ( -18.52830673193259514, 34.28760034481967978, -147.9573921617513577 ) ) ;
#14898 = VECTOR ( 'NONE', #2423, 1000.000000000000000 ) ;
#14899 = CARTESIAN_POINT ( 'NONE',  ( 8.100000000049998761, 34.53220746410000430, -149.5552959529999839 ) ) ;
#14900 = CARTESIAN_POINT ( 'NONE',  ( 12.57628698947108958, 35.71923945894556596, -136.0552959530283772 ) ) ;
#14901 = CARTESIAN_POINT ( 'NONE',  ( -23.55797472130712222, 40.74841938826056520, -146.3388075606171981 ) ) ;
#14902 = CARTESIAN_POINT ( 'NONE',  ( -15.35800208497430930, 33.25688119014312605, -145.9433539410966887 ) ) ;
#14903 = EDGE_CURVE ( 'NONE', #10456, #13256, #9132, .T. ) ;
#14904 = EDGE_CURVE ( 'NONE', #7225, #30, #13173, .T. ) ;
#14905 = CARTESIAN_POINT ( 'NONE',  ( -19.68771884990000132, 32.54972883539999629, -143.8405663050000101 ) ) ;
#14906 = FACE_BOUND ( 'NONE', #6944, .T. ) ;
#14907 = DIRECTION ( 'NONE',  ( 0.000000000000000000, 1.000000000000000000, 0.000000000000000000 ) ) ;
#14908 = ORIENTED_EDGE ( 'NONE', *, *, #10255, .F. ) ;
#14909 = CARTESIAN_POINT ( 'NONE',  ( -5.895487218599030577, 38.46663302055699774, -147.4545603117625205 ) ) ;
#14910 = LINE ( 'NONE', #22520, #11105 ) ;
#14911 = ORIENTED_EDGE ( 'NONE', *, *, #5987, .T. ) ;
#14912 = AXIS2_PLACEMENT_3D ( 'NONE', #4510, #8181, #10326 ) ;
#14913 = EDGE_CURVE ( 'NONE', #20128, #5898, #12768, .T. ) ;
#14914 = EDGE_CURVE ( 'NONE', #2935, #18341, #11854, .T. ) ;
#14915 = CARTESIAN_POINT ( 'NONE',  ( -21.13851658203423867, 36.11334442967607572, -147.9366295169849934 ) ) ;
#14916 = DIRECTION ( 'NONE',  ( 1.000000000000000000, 0.000000000000000000, -1.522591576628786004E-13 ) ) ;
#14917 = ORIENTED_EDGE ( 'NONE', *, *, #2724, .T. ) ;
#14918 = CARTESIAN_POINT ( 'NONE',  ( -13.26154605881311532, 33.84108359974723612, -142.3203849960127627 ) ) ;
#14919 = EDGE_CURVE ( 'NONE', #11360, #18084, #13779, .T. ) ;
#14920 = CARTESIAN_POINT ( 'NONE',  ( -21.35824191591069265, -32.00000000000000000, -141.9623572383524959 ) ) ;
#14921 = ADVANCED_FACE ( 'NONE', ( #19123 ), #10057, .T. ) ;
#14922 = CARTESIAN_POINT ( 'NONE',  ( -13.86630785130000021, -50.50000000000000000, -136.0552959530000123 ) ) ;
#14923 = CARTESIAN_POINT ( 'NONE',  ( -2.499999999839999987, 20.50000000000000000, -140.5552959529999839 ) ) ;
#14924 = CARTESIAN_POINT ( 'NONE',  ( 7.085709294149999060, -13.66851965709999916, -143.5552959529999839 ) ) ;
#14925 = CARTESIAN_POINT ( 'NONE',  ( 4.750000000000000000, -38.23606797749999942, -150.0552959529999839 ) ) ;
#14926 = ORIENTED_EDGE ( 'NONE', *, *, #9924, .F. ) ;
#14927 = CARTESIAN_POINT ( 'NONE',  ( -27.36723106709627729, 36.02973761862455859, -148.4771530685292191 ) ) ;
#14928 = ORIENTED_EDGE ( 'NONE', *, *, #5010, .T. ) ;
#14929 = ORIENTED_EDGE ( 'NONE', *, *, #18339, .T. ) ;
#14930 = CARTESIAN_POINT ( 'NONE',  ( 8.750000000030000891, -42.36803398869999882, -136.0552959530000123 ) ) ;
#14931 = CARTESIAN_POINT ( 'NONE',  ( -9.944031889410000602, 32.62729151690000151, -143.2983400859999961 ) ) ;
#14932 = DIRECTION ( 'NONE',  ( 1.000000000000000000, 0.000000000000000000, -1.526556658859589738E-13 ) ) ;
#14933 = ADVANCED_FACE ( 'NONE', ( #22821 ), #22581, .F. ) ;
#14934 = ORIENTED_EDGE ( 'NONE', *, *, #4379, .F. ) ;
#14935 = LINE ( 'NONE', #2452, #1904 ) ;
#14936 = LINE ( 'NONE', #22306, #5337 ) ;
#14937 = CARTESIAN_POINT ( 'NONE',  ( 31.50000000000000000, -2.273736754430000208E-12, -136.0552959530000123 ) ) ;
#14938 = ORIENTED_EDGE ( 'NONE', *, *, #6605, .F. ) ;
#14939 = CARTESIAN_POINT ( 'NONE',  ( -21.61577042763667578, 39.11111834142336363, -146.9311419176080733 ) ) ;
#14940 = EDGE_CURVE ( 'NONE', #13908, #12438, #6005, .T. ) ;
#14941 = CARTESIAN_POINT ( 'NONE',  ( 9.562417701932698577, 38.05891272967145511, -141.7906281408962172 ) ) ;
#14942 = EDGE_CURVE ( 'NONE', #21515, #4078, #22390, .T. ) ;
#14943 = AXIS2_PLACEMENT_3D ( 'NONE', #1423, #8644, #23184 ) ;
#14944 = DIRECTION ( 'NONE',  ( 0.000000000000000000, 2.257144641399999941E-12, -1.000000000000000000 ) ) ;
#14945 = DIRECTION ( 'NONE',  ( 1.000000000000000000, 0.000000000000000000, 0.000000000000000000 ) ) ;
#14946 = ORIENTED_EDGE ( 'NONE', *, *, #16018, .T. ) ;
#14947 = FACE_OUTER_BOUND ( 'NONE', #13226, .T. ) ;
#14948 = ORIENTED_EDGE ( 'NONE', *, *, #12914, .T. ) ;
#14949 = CARTESIAN_POINT ( 'NONE',  ( 5.740346993226800087, -48.74619218629713657, -150.0552959529999839 ) ) ;
#14950 = ORIENTED_EDGE ( 'NONE', *, *, #14500, .F. ) ;
#14951 = CARTESIAN_POINT ( 'NONE',  ( -27.20920484747068713, 39.08183102471901549, -146.8889507634862071 ) ) ;
#14952 = EDGE_LOOP ( 'NONE', ( #355, #15314, #15706, #18843 ) ) ;
#14953 = CARTESIAN_POINT ( 'NONE',  ( -22.47466675763224231, 32.97119510217613936, -146.3662674461704967 ) ) ;
#14954 = ORIENTED_EDGE ( 'NONE', *, *, #9946, .T. ) ;
#14955 = CARTESIAN_POINT ( 'NONE',  ( -17.99999999999999645, -43.39269908169872991, -150.0552959530000123 ) ) ;
#14956 = ORIENTED_EDGE ( 'NONE', *, *, #18336, .F. ) ;
#14957 = PRODUCT_CONTEXT ( 'NONE', #23319, 'mechanical' ) ;
#14958 = ORIENTED_EDGE ( 'NONE', *, *, #13716, .F. ) ;
#14959 = CARTESIAN_POINT ( 'NONE',  ( 0.000000000000000000, -42.23606797749999942, -150.0552959529999839 ) ) ;
#14960 = CARTESIAN_POINT ( 'NONE',  ( -14.21887350769999969, 37.71951061619999734, -140.5431489169999963 ) ) ;
#14961 = DIRECTION ( 'NONE',  ( 1.000000000000000000, 0.000000000000000000, 0.000000000000000000 ) ) ;
#14962 = DIRECTION ( 'NONE',  ( 0.000000000000000000, -1.000000000000000000, 0.000000000000000000 ) ) ;
#14963 = DIRECTION ( 'NONE',  ( 0.000000000000000000, 1.000000000000000000, 2.245315043809999812E-12 ) ) ;
#14964 = EDGE_CURVE ( 'NONE', #6049, #13387, #7815, .T. ) ;
#14965 = CARTESIAN_POINT ( 'NONE',  ( -7.774431620203307247, 38.87593842133829725, -139.9151280782420486 ) ) ;
#14966 = ORIENTED_EDGE ( 'NONE', *, *, #5903, .F. ) ;
#14967 = LINE ( 'NONE', #13407, #14789 ) ;
#14968 = PLANE ( 'NONE',  #20121 ) ;
#14969 = LINE ( 'NONE', #7702, #21269 ) ;
#14970 = VERTEX_POINT ( 'NONE', #6039 ) ;
#14971 = CARTESIAN_POINT ( 'NONE',  ( 4.499999999879999102, -3.500000000000000000, -136.0552959530000123 ) ) ;
#14972 = CARTESIAN_POINT ( 'NONE',  ( -11.97832217620000073, 39.59660284089999749, -147.8163995769999985 ) ) ;
#14973 = VECTOR ( 'NONE', #20726, 1000.000000000000000 ) ;
#14974 = PLANE ( 'NONE',  #13198 ) ;
#14975 = CARTESIAN_POINT ( 'NONE',  ( 19.13369214859999801, 50.50000000000000000, -136.5552959530000123 ) ) ;
#14976 = VERTEX_POINT ( 'NONE', #4370 ) ;
#14977 = LINE ( 'NONE', #2261, #7512 ) ;
#14978 = CARTESIAN_POINT ( 'NONE',  ( -30.41918043656676574, 40.92081927820395038, -146.2642377558170494 ) ) ;
#14979 = ORIENTED_EDGE ( 'NONE', *, *, #7640, .F. ) ;
#14980 = PLANE ( 'NONE',  #3414 ) ;
#14981 = LINE ( 'NONE', #4277, #4638 ) ;
#14982 = EDGE_LOOP ( 'NONE', ( #3005, #6591, #16961, #16213 ) ) ;
#14983 = PLANE ( 'NONE',  #15142 ) ;
#14984 = CARTESIAN_POINT ( 'NONE',  ( -20.83134323208084027, 41.14286042260535936, -141.6931026970137850 ) ) ;
#14985 = EDGE_LOOP ( 'NONE', ( #18512, #12230, #12543, #9389 ) ) ;
#14986 = CARTESIAN_POINT ( 'NONE',  ( -27.59585739157013151, 36.27528467301697646, -147.4543200874812214 ) ) ;
#14987 = DIRECTION ( 'NONE',  ( 1.457928428160000110E-12, -1.723197716179999783E-12, -1.000000000000000000 ) ) ;
#14988 = EDGE_LOOP ( 'NONE', ( #23465, #16619, #4249, #9333 ) ) ;
#14989 = LINE ( 'NONE', #6067, #5277 ) ;
#14990 = CARTESIAN_POINT ( 'NONE',  ( 4.500000000000000000, -3.500000000000000000, -140.0552959529999839 ) ) ;
#14991 = CYLINDRICAL_SURFACE ( 'NONE', #22037, 6.000000000000004441 ) ;
#14992 = EDGE_LOOP ( 'NONE', ( #3635, #21059, #12814, #10548 ) ) ;
#14993 = ADVANCED_FACE ( 'NONE', ( #8047 ), #19600, .F. ) ;
#14994 = CIRCLE ( 'NONE', #23358, 2.999999999999999112 ) ;
#14995 = CARTESIAN_POINT ( 'NONE',  ( -20.61753010269739406, 36.92891383027767205, -140.0927360959155692 ) ) ;
#14996 = LINE ( 'NONE', #4293, #7898 ) ;
#14997 = EDGE_CURVE ( 'NONE', #6301, #22167, #12116, .T. ) ;
#14998 = ORIENTED_EDGE ( 'NONE', *, *, #6605, .T. ) ;
#14999 = VERTEX_POINT ( 'NONE', #6625 ) ;
#15000 = CARTESIAN_POINT ( 'NONE',  ( -35.47299999999999898, 11.04196010839999964, -143.5552959529999839 ) ) ;
#15001 = CARTESIAN_POINT ( 'NONE',  ( -29.95441468910000182, 40.29796007080000209, -145.3430615500000158 ) ) ;
#15002 = FACE_OUTER_BOUND ( 'NONE', #1652, .T. ) ;
#15003 = CARTESIAN_POINT ( 'NONE',  ( 7.304793568844493379, 36.09237029978162070, -141.7255920985726902 ) ) ;
#15004 = ORIENTED_EDGE ( 'NONE', *, *, #6723, .F. ) ;
#15005 = CARTESIAN_POINT ( 'NONE',  ( -22.52780672249999938, 37.05898997719999954, -140.0074087190000114 ) ) ;
#15006 = LINE ( 'NONE', #11769, #17694 ) ;
#15007 = ADVANCED_FACE ( 'NONE', ( #21509 ), #6861, .F. ) ;
#15008 = DIRECTION ( 'NONE',  ( 4.510774274160000731E-12, -1.321907670990000086E-13, 1.000000000000000000 ) ) ;
#15009 = CARTESIAN_POINT ( 'NONE',  ( 10.68320006080000084, -20.50000000000000000, -150.0552959529999839 ) ) ;
#15010 = CARTESIAN_POINT ( 'NONE',  ( -25.01023491195180881, 37.91851060511771720, -148.1495535101706480 ) ) ;
#15011 = AXIS2_PLACEMENT_3D ( 'NONE', #1214, #15818, #8314 ) ;
#15012 = DIRECTION ( 'NONE',  ( 0.7432941462487078210, 0.000000000000000000, 0.6689647316207368855 ) ) ;
#15013 = CARTESIAN_POINT ( 'NONE',  ( -16.54277457342332269, 34.95491693752516227, -141.0331736024299971 ) ) ;
#15014 = DIRECTION ( 'NONE',  ( 0.000000000000000000, -7.444689577964079813E-14, -1.000000000000000000 ) ) ;
#15015 = PLANE ( 'NONE',  #7662 ) ;
#15016 = CARTESIAN_POINT ( 'NONE',  ( 8.750000000000000000, -39.23606797749999942, -150.0552959529999839 ) ) ;
#15017 = ORIENTED_EDGE ( 'NONE', *, *, #3884, .F. ) ;
#15018 = CARTESIAN_POINT ( 'NONE',  ( -6.183234097834880316, 41.28010592191888151, -143.5033826244021782 ) ) ;
#15019 = DIRECTION ( 'NONE',  ( 5.094701932209999624E-24, 1.000000000000000000, -1.149947916579999802E-35 ) ) ;
#15020 = VERTEX_POINT ( 'NONE', #5317 ) ;
#15022 = AXIS2_PLACEMENT_3D ( 'NONE', #5004, #12249, #8321 ) ;
#15021 = CARTESIAN_POINT ( 'NONE',  ( -23.19912457534285366, 34.77544957999561603, -141.0327754292524389 ) ) ;
#15023 = VECTOR ( 'NONE', #5439, 1000.000000000000000 ) ;
#15024 = DIRECTION ( 'NONE',  ( 2.257157423930000049E-12, 0.000000000000000000, 1.000000000000000000 ) ) ;
#15025 = ORIENTED_EDGE ( 'NONE', *, *, #19867, .T. ) ;
#15026 = CARTESIAN_POINT ( 'NONE',  ( -12.58047663530000015, 34.35960099889999952, -147.8017659109999897 ) ) ;
#15027 = FACE_OUTER_BOUND ( 'NONE', #14605, .T. ) ;
#15028 = EDGE_CURVE ( 'NONE', #8147, #22250, #8751, .T. ) ;
#15029 = DIRECTION ( 'NONE',  ( 0.000000000000000000, 7.657380550038349542E-13, -1.000000000000000000 ) ) ;
#15030 = CARTESIAN_POINT ( 'NONE',  ( 8.500000000050000892, 37.00000000000000000, -149.5552959529999839 ) ) ;
#15031 = CARTESIAN_POINT ( 'NONE',  ( 3.999999999879999546, -4.750000000000000000, -135.0552959530000123 ) ) ;
#15032 = CARTESIAN_POINT ( 'NONE',  ( -25.86630785129999666, -2.273736754430000208E-12, -136.0552959530000123 ) ) ;
#15033 = ORIENTED_EDGE ( 'NONE', *, *, #9279, .F. ) ;
#15034 = CARTESIAN_POINT ( 'NONE',  ( -28.42317279839999955, 33.35748734759999934, -144.4144508710000139 ) ) ;
#15035 = ORIENTED_EDGE ( 'NONE', *, *, #12973, .F. ) ;
#15036 = EDGE_CURVE ( 'NONE', #3155, #14150, #21524, .T. ) ;
#15037 = ADVANCED_FACE ( 'NONE', ( #17693 ), #17809, .F. ) ;
#15038 = ORIENTED_EDGE ( 'NONE', *, *, #14608, .T. ) ;
#15039 = VECTOR ( 'NONE', #1656, 1000.000000000000000 ) ;
#15040 = CARTESIAN_POINT ( 'NONE',  ( -6.033650297970000409, 36.94170754819999303, -147.9652040070000112 ) ) ;
#15041 = CARTESIAN_POINT ( 'NONE',  ( 23.99773978629999860, -29.25880395889999974, -148.5552959529999839 ) ) ;
#15042 = VECTOR ( 'NONE', #13589, 1000.000000000000000 ) ;
#15043 = DIRECTION ( 'NONE',  ( -1.000000000000000000, 0.000000000000000000, 0.000000000000000000 ) ) ;
#15044 = EDGE_CURVE ( 'NONE', #9795, #11233, #7927, .T. ) ;
#15045 = ORIENTED_EDGE ( 'NONE', *, *, #21016, .T. ) ;
#15046 = CARTESIAN_POINT ( 'NONE',  ( -35.07300000000000040, 14.00000000000000000, -144.5552959529999839 ) ) ;
#15047 = EDGE_CURVE ( 'NONE', #8241, #19376, #3413, .T. ) ;
#15048 = DIRECTION ( 'NONE',  ( 3.994014902950000436E-29, -1.000000000000000000, 4.148443855749999753E-27 ) ) ;
#15049 = ORIENTED_EDGE ( 'NONE', *, *, #1973, .T. ) ;
#15050 = CARTESIAN_POINT ( 'NONE',  ( -21.19005019800000156, 41.30866696430000218, -143.6114845980000041 ) ) ;
#15051 = CARTESIAN_POINT ( 'NONE',  ( 9.568800768469639451, 38.05246265392671745, -141.7876273308280872 ) ) ;
#15052 = CARTESIAN_POINT ( 'NONE',  ( -2.499999999859999988, 20.50000000000000000, -147.0552959529999839 ) ) ;
#15053 = EDGE_CURVE ( 'NONE', #19299, #14651, #21159, .T. ) ;
#15054 = VECTOR ( 'NONE', #20276, 1000.000000000000000 ) ;
#15055 = FACE_OUTER_BOUND ( 'NONE', #22366, .T. ) ;
#15056 = AXIS2_PLACEMENT_3D ( 'NONE', #6717, #13978, #21249 ) ;
#15057 = VERTEX_POINT ( 'NONE', #21629 ) ;
#15058 = EDGE_CURVE ( 'NONE', #10920, #22442, #10768, .T. ) ;
#15059 = CARTESIAN_POINT ( 'NONE',  ( 24.41610067590000099, -29.22497285029999858, -144.5552959529999839 ) ) ;
#15060 = ORIENTED_EDGE ( 'NONE', *, *, #16241, .T. ) ;
#15061 = DIRECTION ( 'NONE',  ( 2.257749542879999954E-12, 0.000000000000000000, 1.000000000000000000 ) ) ;
#15062 = ORIENTED_EDGE ( 'NONE', *, *, #15905, .T. ) ;
#15063 = CARTESIAN_POINT ( 'NONE',  ( -25.95437585267248082, 39.65968214943575987, -140.4458241776663954 ) ) ;
#15064 = ADVANCED_FACE ( 'NONE', ( #1181 ), #10653, .T. ) ;
#15065 = ORIENTED_EDGE ( 'NONE', *, *, #12652, .T. ) ;
#15066 = DIRECTION ( 'NONE',  ( 2.257305453670000045E-12, 0.000000000000000000, 1.000000000000000000 ) ) ;
#15067 = EDGE_CURVE ( 'NONE', #11916, #683, #5409, .T. ) ;
#15068 = ORIENTED_EDGE ( 'NONE', *, *, #7473, .F. ) ;
#15069 = CARTESIAN_POINT ( 'NONE',  ( -12.60099947280544797, -44.84364015992472474, -150.0552959529999555 ) ) ;
#15070 = ORIENTED_EDGE ( 'NONE', *, *, #13674, .F. ) ;
#15071 = EDGE_CURVE ( 'NONE', #16883, #18382, #12212, .T. ) ;
#15072 = VERTEX_POINT ( 'NONE', #10417 ) ;
#15073 = CARTESIAN_POINT ( 'NONE',  ( -27.77832206610000298, 37.03059619289999915, -147.6270870419999710 ) ) ;
#15074 = CARTESIAN_POINT ( 'NONE',  ( -15.00140173379999986, 40.20535686069999315, -145.8913236320000237 ) ) ;
#15075 = AXIS2_PLACEMENT_3D ( 'NONE', #18265, #14576, #16124 ) ;
#15076 = DIRECTION ( 'NONE',  ( 0.6459422414661339928, 0.7633862853691482098, 0.000000000000000000 ) ) ;
#15077 = CARTESIAN_POINT ( 'NONE',  ( -7.010349701930000066, 37.05829245179999987, -148.1453878979999956 ) ) ;
#15078 = CARTESIAN_POINT ( 'NONE',  ( -6.227860603739999945, 35.34754625490000279, -147.7419925389999946 ) ) ;
#15079 = CARTESIAN_POINT ( 'NONE',  ( -8.514310886032820491, 36.94123471670531700, -140.1199228274701909 ) ) ;
#15080 = EDGE_LOOP ( 'NONE', ( #5648, #16285, #7887, #17944 ) ) ;
#15081 = LINE ( 'NONE', #6036, #7553 ) ;
#15082 = DIRECTION ( 'NONE',  ( -1.211690350419999855E-27, -2.765629237170000203E-27, 1.000000000000000000 ) ) ;
#15083 = CARTESIAN_POINT ( 'NONE',  ( -26.39607007120000048, 36.95534867429999792, -140.3840478969999879 ) ) ;
#15084 = ORIENTED_EDGE ( 'NONE', *, *, #21376, .F. ) ;
#15085 = VECTOR ( 'NONE', #1500, 1000.000000000000000 ) ;
#15086 = CARTESIAN_POINT ( 'NONE',  ( -10.86836323999999898, 38.91206754959999614, -139.9811931129999891 ) ) ;
#15087 = CARTESIAN_POINT ( 'NONE',  ( -18.22769797923110957, 36.96487028399720742, -148.6596776398728821 ) ) ;
#15088 = DIRECTION ( 'NONE',  ( 0.000000000000000000, -2.256894259950000208E-12, 1.000000000000000000 ) ) ;
#15089 = CIRCLE ( 'NONE', #3322, 1.499999999999999556 ) ;
#15090 = VERTEX_POINT ( 'NONE', #1402 ) ;
#15091 = CARTESIAN_POINT ( 'NONE',  ( -7.324031428439999658, 35.31041870520000003, -140.2046280479999893 ) ) ;
#15092 = DIRECTION ( 'NONE',  ( 2.257157423930000049E-12, 0.000000000000000000, 1.000000000000000000 ) ) ;
#15093 = ORIENTED_EDGE ( 'NONE', *, *, #9897, .F. ) ;
#15094 = FACE_BOUND ( 'NONE', #21686, .T. ) ;
#15095 = CARTESIAN_POINT ( 'NONE',  ( -27.97684248819999908, 35.51254237909999745, -147.4365014880000047 ) ) ;
#15096 = ADVANCED_FACE ( 'NONE', ( #23168 ), #8626, .F. ) ;
#15097 = ORIENTED_EDGE ( 'NONE', *, *, #19785, .F. ) ;
#15098 = CARTESIAN_POINT ( 'NONE',  ( -6.683153925719999222, -50.50000000000000000, -150.0552959529999839 ) ) ;
#15099 = EDGE_CURVE ( 'NONE', #22094, #14626, #21865, .T. ) ;
#15100 = CARTESIAN_POINT ( 'NONE',  ( -21.42908239836678774, 38.93534789603918966, -148.4669439360840784 ) ) ;
#15101 = ORIENTED_EDGE ( 'NONE', *, *, #19045, .F. ) ;
#15102 = CARTESIAN_POINT ( 'NONE',  ( -32.50000000000000000, 51.50000000000000000, -142.8052959529999839 ) ) ;
#15103 = VERTEX_POINT ( 'NONE', #2106 ) ;
#15104 = FACE_BOUND ( 'NONE', #16836, .T. ) ;
#15105 = FACE_OUTER_BOUND ( 'NONE', #12582, .T. ) ;
#15106 = CARTESIAN_POINT ( 'NONE',  ( 32.00000000000000000, -33.03620104880000241, -136.0552959530000123 ) ) ;
#15107 = VECTOR ( 'NONE', #18700, 1000.000000000000000 ) ;
#15108 = EDGE_LOOP ( 'NONE', ( #20260, #5515 ) ) ;
#15109 = FACE_BOUND ( 'NONE', #17110, .T. ) ;
#15110 = VECTOR ( 'NONE', #10315, 1000.000000000000000 ) ;
#15111 = PLANE ( 'NONE',  #1860 ) ;
#15112 = ORIENTED_EDGE ( 'NONE', *, *, #2189, .T. ) ;
#15113 = VERTEX_POINT ( 'NONE', #20196 ) ;
#15114 = SHAPE_REPRESENTATION ( 'Main Base', ( #5025 ), #8794 ) ;
#15115 = CARTESIAN_POINT ( 'NONE',  ( 22.40528270640000130, -21.39206583629999869, -145.5552959529999839 ) ) ;
#15116 = CARTESIAN_POINT ( 'NONE',  ( 18.95053822279999878, -50.00000000000000000, -151.0552959529999839 ) ) ;
#15117 = CARTESIAN_POINT ( 'NONE',  ( 17.66940543669999997, -18.68690163239999791, -144.5552959529999839 ) ) ;
#15118 = CARTESIAN_POINT ( 'NONE',  ( 7.500784825167067460, 35.87811771440581765, -141.8201969968949925 ) ) ;
#15119 = ORIENTED_EDGE ( 'NONE', *, *, #11527, .F. ) ;
#15120 = SURFACE_STYLE_USAGE ( .BOTH. , #18809 ) ;
#15121 = LINE ( 'NONE', #11422, #10454 ) ;
#15122 = EDGE_CURVE ( 'NONE', #7449, #16762, #14704, .T. ) ;
#15123 = AXIS2_PLACEMENT_3D ( 'NONE', #14461, #8284, #15558 ) ;
#15124 = CARTESIAN_POINT ( 'NONE',  ( -13.53835085784080761, -42.60938321240698201, -150.0552959529999839 ) ) ;
#15125 = PLANE ( 'NONE',  #9923 ) ;
#15126 = EDGE_CURVE ( 'NONE', #7237, #2371, #6770, .T. ) ;
#15127 = CARTESIAN_POINT ( 'NONE',  ( -24.22314457607379623, 36.96432676151304264, -148.6204621725955519 ) ) ;
#15128 = AXIS2_PLACEMENT_3D ( 'NONE', #2576, #15411, #22670 ) ;
#15129 = EDGE_CURVE ( 'NONE', #6192, #903, #2002, .T. ) ;
#15130 = CARTESIAN_POINT ( 'NONE',  ( -15.57039528535599970, 36.22627288623296238, -147.5570433397527665 ) ) ;
#15131 = CARTESIAN_POINT ( 'NONE',  ( -16.48516879800526169, 34.41988679506793858, -147.5123417674411144 ) ) ;
#15132 = LINE ( 'NONE', #9641, #20591 ) ;
#15133 = CARTESIAN_POINT ( 'NONE',  ( 4.374398326270000581, -26.09174856970000178, -143.5552959529999839 ) ) ;
#15134 = DIRECTION ( 'NONE',  ( -0.1146332952500066227, -0.9934078757590583120, -1.023181539490060155E-13 ) ) ;
#15135 = ORIENTED_EDGE ( 'NONE', *, *, #11609, .T. ) ;
#15136 = CARTESIAN_POINT ( 'NONE',  ( -5.450498087531185476, 40.62522382734958626, -144.4475518853465701 ) ) ;
#15137 = FACE_BOUND ( 'NONE', #7719, .T. ) ;
#15138 = ORIENTED_EDGE ( 'NONE', *, *, #21566, .T. ) ;
#15139 = CYLINDRICAL_SURFACE ( 'NONE', #11428, 0.5000000000000079936 ) ;
#15140 = EDGE_CURVE ( 'NONE', #7002, #10448, #9327, .T. ) ;
#15141 = AXIS2_PLACEMENT_3D ( 'NONE', #607, #13551, #15238 ) ;
#15142 = AXIS2_PLACEMENT_3D ( 'NONE', #22478, #2499, #22243 ) ;
#15143 = CARTESIAN_POINT ( 'NONE',  ( -22.21135766849999982, 35.30661492690000358, -147.9492090369999744 ) ) ;
#15144 = DIRECTION ( 'NONE',  ( 2.257157423930000049E-12, 0.000000000000000000, 1.000000000000000000 ) ) ;
#15145 = EDGE_LOOP ( 'NONE', ( #10511, #19855, #16009, #18285 ) ) ;
#15146 = CARTESIAN_POINT ( 'NONE',  ( -12.64961778247436897, 33.30795510890303746, -144.5205897159969481 ) ) ;
#15147 = DIRECTION ( 'NONE',  ( -0.1435602414469281940, -0.9896415801065048257, 3.849849731938073961E-13 ) ) ;
#15148 = CIRCLE ( 'NONE', #7909, 8.176568160360000448 ) ;
#15149 = DIRECTION ( 'NONE',  ( 0.7432941462487078210, 0.000000000000000000, 0.6689647316207368855 ) ) ;
#15150 = DIRECTION ( 'NONE',  ( 0.000000000000000000, -2.257144641399999941E-12, -1.000000000000000000 ) ) ;
#15151 = CARTESIAN_POINT ( 'NONE',  ( -3.500000000000000000, 40.00000000000000000, -151.0552959529999839 ) ) ;
#15152 = CARTESIAN_POINT ( 'NONE',  ( 3.190250522981681769, -4.257526301755348186, -136.0552959530071746 ) ) ;
#15153 = ADVANCED_FACE ( 'NONE', ( #14484 ), #5548, .T. ) ;
#15154 = ORIENTED_EDGE ( 'NONE', *, *, #2589, .T. ) ;
#15155 = EDGE_CURVE ( 'NONE', #20206, #17461, #3651, .T. ) ;
#15156 = CARTESIAN_POINT ( 'NONE',  ( -28.06178240312047834, 37.06443177824845492, -147.7991814974922420 ) ) ;
#15157 = VECTOR ( 'NONE', #22688, 1000.000000000000000 ) ;
#15158 =( LENGTH_UNIT ( ) NAMED_UNIT ( * ) SI_UNIT ( .MILLI., .METRE. ) );
#15159 = VECTOR ( 'NONE', #14547, 1000.000000000000000 ) ;
#15160 = ORIENTED_EDGE ( 'NONE', *, *, #20971, .T. ) ;
#15161 = CARTESIAN_POINT ( 'NONE',  ( -14.58163105951714655, 36.93319896292500459, -139.6872257169340514 ) ) ;
#15162 = DIRECTION ( 'NONE',  ( -2.507771768019999718E-12, 0.000000000000000000, 1.000000000000000000 ) ) ;
#15163 = DIRECTION ( 'NONE',  ( 0.000000000000000000, -2.256894259950000208E-12, 1.000000000000000000 ) ) ;
#15164 = CIRCLE ( 'NONE', #3772, 35.00000000000000000 ) ;
#15165 = ORIENTED_EDGE ( 'NONE', *, *, #1065, .F. ) ;
#15166 = VECTOR ( 'NONE', #5920, 1000.000000000000000 ) ;
#15167 = CARTESIAN_POINT ( 'NONE',  ( -32.50000000000000000, 21.50000000000000000, -136.5552959530000123 ) ) ;
#15168 = EDGE_CURVE ( 'NONE', #14075, #6228, #4395, .T. ) ;
#15169 = CARTESIAN_POINT ( 'NONE',  ( -30.02199999990000023, 40.03108891319999429, -145.8052959529999839 ) ) ;
#15170 = ORIENTED_EDGE ( 'NONE', *, *, #11263, .F. ) ;
#15171 = CARTESIAN_POINT ( 'NONE',  ( -20.66421688137213053, 40.12815996892139481, -145.9609113517520029 ) ) ;
#15172 = CARTESIAN_POINT ( 'NONE',  ( 9.720672476820208630, 37.87260413900303746, -141.7122832975126414 ) ) ;
#15173 = FACE_BOUND ( 'NONE', #14888, .T. ) ;
#15174 = CIRCLE ( 'NONE', #17448, 35.00000000000000000 ) ;
#15175 = EDGE_CURVE ( 'NONE', #2933, #17870, #22254, .T. ) ;
#15176 = CARTESIAN_POINT ( 'NONE',  ( 22.68320006080000084, -34.50000000000000000, -149.3052959529999839 ) ) ;
#15177 = CIRCLE ( 'NONE', #5312, 5.000000000000000000 ) ;
#15178 = CARTESIAN_POINT ( 'NONE',  ( -25.55414838373298991, 33.45093896582719140, -143.7269752718342488 ) ) ;
#15179 = ORIENTED_EDGE ( 'NONE', *, *, #6854, .F. ) ;
#15180 = VECTOR ( 'NONE', #9214, 1000.000000000000000 ) ;
#15181 = VECTOR ( 'NONE', #18858, 1000.000000000000000 ) ;
#15182 = VECTOR ( 'NONE', #7492, 1000.000000000000000 ) ;
#15183 = DIRECTION ( 'NONE',  ( 0.000000000000000000, 0.000000000000000000, 1.000000000000000000 ) ) ;
#15184 = ORIENTED_EDGE ( 'NONE', *, *, #5183, .T. ) ;
#15185 = PLANE ( 'NONE',  #2597 ) ;
#15186 = EDGE_CURVE ( 'NONE', #8234, #11634, #12748, .T. ) ;
#15187 = ORIENTED_EDGE ( 'NONE', *, *, #12943, .F. ) ;
#15188 = CARTESIAN_POINT ( 'NONE',  ( -27.29941367908698524, 38.43084994578902069, -147.2672509616508307 ) ) ;
#15189 = ORIENTED_EDGE ( 'NONE', *, *, #16227, .F. ) ;
#15190 = DIRECTION ( 'NONE',  ( 1.000000000000000000, 0.000000000000000000, 0.000000000000000000 ) ) ;
#15191 = ORIENTED_EDGE ( 'NONE', *, *, #826, .T. ) ;
#15192 = CARTESIAN_POINT ( 'NONE',  ( 1.352544480119999948, -20.86379603889999856, -146.5552959529999839 ) ) ;
#15193 = VERTEX_POINT ( 'NONE', #20307 ) ;
#15194 = EDGE_LOOP ( 'NONE', ( #22800, #15310, #18942, #6155 ) ) ;
#15195 = CARTESIAN_POINT ( 'NONE',  ( -27.90252014676526926, 38.00321959428593743, -148.5304241855687906 ) ) ;
#15196 = EDGE_CURVE ( 'NONE', #21201, #5099, #3640, .T. ) ;
#15197 = CARTESIAN_POINT ( 'NONE',  ( 25.38675467179999856, 45.20894709569999748, -149.5552959529999839 ) ) ;
#15198 = FACE_OUTER_BOUND ( 'NONE', #16316, .T. ) ;
#15199 = CARTESIAN_POINT ( 'NONE',  ( -32.50000000000000000, 51.50000000000000000, -149.5552959529999839 ) ) ;
#15200 = VECTOR ( 'NONE', #8447, 1000.000000000000000 ) ;
#15201 = VECTOR ( 'NONE', #16837, 1000.000000000000000 ) ;
#15202 = CARTESIAN_POINT ( 'NONE',  ( -6.697072761360190363, 32.84210578784889378, -146.5313758896071477 ) ) ;
#15203 = AXIS2_PLACEMENT_3D ( 'NONE', #13395, #20321, #20665 ) ;
#15204 = CARTESIAN_POINT ( 'NONE',  ( -8.585705256233374882, 39.77515751163792146, -140.1536556790775023 ) ) ;
#15205 = AXIS2_PLACEMENT_3D ( 'NONE', #21884, #18186, #23194 ) ;
#15206 = EDGE_LOOP ( 'NONE', ( #17680, #15393, #20100, #8169 ) ) ;
#15207 = FACE_OUTER_BOUND ( 'NONE', #18005, .T. ) ;
#15208 = EDGE_CURVE ( 'NONE', #3901, #11841, #14830, .T. ) ;
#15209 = CARTESIAN_POINT ( 'NONE',  ( -9.347107914279998653, -17.32706600430000066, -144.5552959529999839 ) ) ;
#15210 = EDGE_CURVE ( 'NONE', #802, #9566, #14596, .T. ) ;
#15211 = DIRECTION ( 'NONE',  ( 0.000000000000000000, -1.000000000000000000, 0.000000000000000000 ) ) ;
#15212 = ORIENTED_EDGE ( 'NONE', *, *, #8806, .T. ) ;
#15213 = EDGE_CURVE ( 'NONE', #4470, #12346, #10886, .T. ) ;
#15214 = CARTESIAN_POINT ( 'NONE',  ( -12.45288479873165954, 40.94156371644511694, -144.5313000001702619 ) ) ;
#15215 = EDGE_CURVE ( 'NONE', #4709, #2330, #1880, .T. ) ;
#15216 = FACE_OUTER_BOUND ( 'NONE', #8422, .T. ) ;
#15217 = LINE ( 'NONE', #7820, #20202 ) ;
#15218 = ORIENTED_EDGE ( 'NONE', *, *, #13034, .T. ) ;
#15219 =( LENGTH_UNIT ( ) NAMED_UNIT ( * ) SI_UNIT ( .MILLI., .METRE. ) );
#15220 = LINE ( 'NONE', #22588, #6307 ) ;
#15221 = VECTOR ( 'NONE', #16423, 1000.000000000000000 ) ;
#15222 = VECTOR ( 'NONE', #14592, 1000.000000000000000 ) ;
#15223 = ORIENTED_EDGE ( 'NONE', *, *, #5720, .F. ) ;
#15224 = DIRECTION ( 'NONE',  ( -0.1435602414469281940, -0.9896415801065047146, 3.835814712303428266E-13 ) ) ;
#15225 = CARTESIAN_POINT ( 'NONE',  ( 12.94820732169999999, -17.45719265660000019, -148.5552959529999839 ) ) ;
#15226 = ORIENTED_EDGE ( 'NONE', *, *, #15047, .F. ) ;
#15227 = CARTESIAN_POINT ( 'NONE',  ( -31.50000000000000000, -50.00000000000000000, -149.5552959529999839 ) ) ;
#15228 = CARTESIAN_POINT ( 'NONE',  ( -20.32722469806098076, 41.69472958972785648, -143.6736157908201790 ) ) ;
#15229 = VERTEX_POINT ( 'NONE', #11230 ) ;
#15230 = CARTESIAN_POINT ( 'NONE',  ( -28.24106514979908056, 36.25312149646672566, -140.0297965533989384 ) ) ;
#15231 = DIRECTION ( 'NONE',  ( -0.9850838563818458127, 0.1720749717299729642, 4.465905845959301396E-12 ) ) ;
#15232 = ORIENTED_EDGE ( 'NONE', *, *, #2358, .T. ) ;
#15233 = DIRECTION ( 'NONE',  ( 0.7633862853691523176, 0.6459422414661291079, -1.722923451730345384E-12 ) ) ;
#15234 = DIRECTION ( 'NONE',  ( 0.000000000000000000, -1.000000000000000000, 0.000000000000000000 ) ) ;
#15235 = DIRECTION ( 'NONE',  ( -0.7071067811865471286, -0.7071067811865477948, 1.595945597898661113E-12 ) ) ;
#15236 = EDGE_LOOP ( 'NONE', ( #12350, #8967, #16075, #18894, #9685, #8146 ) ) ;
#15237 = FACE_OUTER_BOUND ( 'NONE', #17644, .T. ) ;
#15238 = DIRECTION ( 'NONE',  ( 0.000000000000000000, 5.873289694040000105E-29, -1.000000000000000000 ) ) ;
#15239 = VERTEX_POINT ( 'NONE', #18504 ) ;
#15240 = VECTOR ( 'NONE', #1833, 1000.000000000000000 ) ;
#15241 = EDGE_CURVE ( 'NONE', #15634, #18790, #20068, .T. ) ;
#15242 = ORIENTED_EDGE ( 'NONE', *, *, #21919, .T. ) ;
#15243 = LINE ( 'NONE', #8193, #12395 ) ;
#15244 = CARTESIAN_POINT ( 'NONE',  ( -30.02199999990000023, 40.03108891319999429, -145.8052959529999839 ) ) ;
#15245 = CARTESIAN_POINT ( 'NONE',  ( -5.316799939240000938, 0.9999999999989999111, -148.5552959529999839 ) ) ;
#15246 = CARTESIAN_POINT ( 'NONE',  ( 23.41308733940000053, -15.43505800149999985, -148.5552959529999839 ) ) ;
#15247 = VERTEX_POINT ( 'NONE', #11012 ) ;
#15248 = LINE ( 'NONE', #20261, #9385 ) ;
#15249 = PLANE ( 'NONE',  #8556 ) ;
#15250 = CARTESIAN_POINT ( 'NONE',  ( -16.20085980602537035, -42.08011361693860408, -150.0552959529999839 ) ) ;
#15251 = CARTESIAN_POINT ( 'NONE',  ( -30.49999999990000177, 26.50000000000000000, -148.3052959529999839 ) ) ;
#15252 = CARTESIAN_POINT ( 'NONE',  ( -24.46575914854654243, 41.11257952955785555, -146.4371654771300086 ) ) ;
#15253 = AXIS2_PLACEMENT_3D ( 'NONE', #6011, #15856, #4918 ) ;
#15254 = CLOSED_SHELL ( 'NONE', ( #7358, #18707, #12671, #20218, #1561, #9351, #17984, #7997, #10793, #13470, #13819, #10031, #4727, #3880, #17463, #15007 ) ) ;
#15255 = AXIS2_PLACEMENT_3D ( 'NONE', #11110, #19937, #5645 ) ;
#15256 = CARTESIAN_POINT ( 'NONE',  ( 9.810375642909303195, -19.99460661104259884, -148.5552959529999555 ) ) ;
#15257 = DIRECTION ( 'NONE',  ( 3.994014902950000436E-29, -1.000000000000000000, 4.148443855749999753E-27 ) ) ;
#15258 = CARTESIAN_POINT ( 'NONE',  ( 16.22102609572369758, -22.92413991441253529, -146.5552959530244834 ) ) ;
#15259 = CARTESIAN_POINT ( 'NONE',  ( 23.50000000000000000, -20.50000000000000000, -143.5552959529999839 ) ) ;
#15260 = CARTESIAN_POINT ( 'NONE',  ( -15.00000000000000000, -43.00000000000000000, -137.0552959530000123 ) ) ;
#15261 = ORIENTED_EDGE ( 'NONE', *, *, #9231, .T. ) ;
#15262 = CARTESIAN_POINT ( 'NONE',  ( -9.697321561110106458, 33.26273935370599588, -144.1849952531234180 ) ) ;
#15263 = DIRECTION ( 'NONE',  ( 1.000000000000000000, -5.094701932209999624E-24, 0.000000000000000000 ) ) ;
#15264 = APPLICATION_CONTEXT ( 'automotive_design' ) ;
#15265 = EDGE_LOOP ( 'NONE', ( #14017, #4110, #20287, #841 ) ) ;
#15266 =( BOUNDED_CURVE ( )  B_SPLINE_CURVE ( 5, ( #6558, #13825, #8455, #10113, #21088, #13699 ),
 .UNSPECIFIED., .F., .F. ) 
 B_SPLINE_CURVE_WITH_KNOTS ( ( 6, 6 ),
 ( 1.570796326447242430, 3.141592653590000062 ),
 .UNSPECIFIED. ) 
 CURVE ( )  GEOMETRIC_REPRESENTATION_ITEM ( )  RATIONAL_B_SPLINE_CURVE ( ( 0.2500000000000000000, 0.2499999999557221131, 0.2999999999335831724, 0.3999999999114442484, 0.5999999999114442595, 1.000000000000000000 ) ) 
 REPRESENTATION_ITEM ( '' )  );
#15267 = FILL_AREA_STYLE ('',( #7987 ) ) ;
#15268 = EDGE_CURVE ( 'NONE', #4135, #19589, #2223, .T. ) ;
#15269 = FACE_OUTER_BOUND ( 'NONE', #7561, .T. ) ;
#15270 = VECTOR ( 'NONE', #16188, 1000.000000000000000 ) ;
#15271 = AXIS2_PLACEMENT_3D ( 'NONE', #5849, #163, #18585 ) ;
#15272 = CARTESIAN_POINT ( 'NONE',  ( 6.499999999879999102, -4.000000000000000000, -135.4552959529999896 ) ) ;
#15273 = VERTEX_POINT ( 'NONE', #20768 ) ;
#15274 = AXIS2_PLACEMENT_3D ( 'NONE', #7054, #7404, #7515 ) ;
#15275 = CARTESIAN_POINT ( 'NONE',  ( -13.60030749279999895, 34.19157895370000233, -140.3499153360000093 ) ) ;
#15276 = CARTESIAN_POINT ( 'NONE',  ( -16.35051094565787366, 37.08015310164943656, -139.9332297720364977 ) ) ;
#15277 = DIRECTION ( 'NONE',  ( 2.257749542879999954E-12, 0.000000000000000000, 1.000000000000000000 ) ) ;
#15278 = CARTESIAN_POINT ( 'NONE',  ( 5.749999999879999102, -4.000000000000000000, -135.4552959529999896 ) ) ;
#15279 = LINE ( 'NONE', #2667, #16988 ) ;
#15280 = CARTESIAN_POINT ( 'NONE',  ( -9.072898850179999641, 36.94639249900000522, -148.2684494029999769 ) ) ;
#15281 = CARTESIAN_POINT ( 'NONE',  ( -7.828824709450000086, 39.51093879980000168, -140.6700787229999889 ) ) ;
#15282 = ORIENTED_EDGE ( 'NONE', *, *, #20813, .T. ) ;
#15283 = DIRECTION ( 'NONE',  ( 0.000000000000000000, -1.000000000000000000, 0.000000000000000000 ) ) ;
#15284 =( LENGTH_UNIT ( ) NAMED_UNIT ( * ) SI_UNIT ( .MILLI., .METRE. ) );
#15285 = ORIENTED_EDGE ( 'NONE', *, *, #22728, .T. ) ;
#15286 = CARTESIAN_POINT ( 'NONE',  ( -14.47796399077968310, 35.98708302378778967, -139.7013159814367782 ) ) ;
#15287 = CARTESIAN_POINT ( 'NONE',  ( 19.77963439019999825, -51.26338628519999929, -136.0552959519999945 ) ) ;
#15288 = VECTOR ( 'NONE', #8762, 1000.000000000000000 ) ;
#15289 = CIRCLE ( 'NONE', #2292, 1.000000000000000888 ) ;
#15290 = DIRECTION ( 'NONE',  ( 1.000000000000000000, 0.000000000000000000, 0.000000000000000000 ) ) ;
#15291 = ORIENTED_EDGE ( 'NONE', *, *, #22038, .T. ) ;
#15292 = DIRECTION ( 'NONE',  ( -2.507771768019999718E-12, 0.000000000000000000, 1.000000000000000000 ) ) ;
#15293 = CARTESIAN_POINT ( 'NONE',  ( 11.68320006079999906, -20.50000000000000000, -150.0552959529999839 ) ) ;
#15294 = ORIENTED_EDGE ( 'NONE', *, *, #7178, .F. ) ;
#15295 = CARTESIAN_POINT ( 'NONE',  ( -20.41826969035592754, 40.54732898170615840, -143.7678329423778223 ) ) ;
#15296 = EDGE_CURVE ( 'NONE', #18780, #10634, #4463, .T. ) ;
#15297 = CARTESIAN_POINT ( 'NONE',  ( -18.28711887264178060, 38.42777126315955627, -147.2271535123214790 ) ) ;
#15298 = ADVANCED_FACE ( 'NONE', ( #6007 ), #13617, .T. ) ;
#15299 = DIRECTION ( 'NONE',  ( -1.701177084980000217E-20, -4.426606872460000157E-37, -1.000000000000000000 ) ) ;
#15300 = CARTESIAN_POINT ( 'NONE',  ( -21.35824191589999899, -4.000000000000000000, -141.0657682190000060 ) ) ;
#15301 = CARTESIAN_POINT ( 'NONE',  ( -25.27079369000000142, 34.74837955689999802, -147.2605407199999945 ) ) ;
#15302 = VERTEX_POINT ( 'NONE', #20537 ) ;
#15303 = VECTOR ( 'NONE', #21210, 1000.000000000000000 ) ;
#15304 = FACE_OUTER_BOUND ( 'NONE', #21020, .T. ) ;
#15305 = ORIENTED_EDGE ( 'NONE', *, *, #20945, .T. ) ;
#15306 = DIRECTION ( 'NONE',  ( 5.094701932209999624E-24, 1.000000000000000000, -1.149947916579999802E-35 ) ) ;
#15307 = ORIENTED_EDGE ( 'NONE', *, *, #8554, .T. ) ;
#15308 = EDGE_LOOP ( 'NONE', ( #5582, #9760, #782, #20407 ) ) ;
#15309 = CARTESIAN_POINT ( 'NONE',  ( -18.07392865170000107, -1.500000000000000000, -147.3157682190000060 ) ) ;
#15310 = ORIENTED_EDGE ( 'NONE', *, *, #5415, .F. ) ;
#15311 = CARTESIAN_POINT ( 'NONE',  ( -23.18315392570000100, 51.50000000000000000, -137.0552959530000123 ) ) ;
#15312 = ORIENTED_EDGE ( 'NONE', *, *, #14006, .T. ) ;
#15313 = EDGE_CURVE ( 'NONE', #2866, #10602, #1023, .T. ) ;
#15314 = ORIENTED_EDGE ( 'NONE', *, *, #16076, .F. ) ;
#15315 = DIRECTION ( 'NONE',  ( 0.000000000000000000, 0.000000000000000000, 1.000000000000000000 ) ) ;
#15316 = CYLINDRICAL_SURFACE ( 'NONE', #11390, 0.7499999999999997780 ) ;
#15317 = DIRECTION ( 'NONE',  ( 0.000000000000000000, 1.000000000000000000, 0.000000000000000000 ) ) ;
#15318 =( GEOMETRIC_REPRESENTATION_CONTEXT ( 3 ) GLOBAL_UNCERTAINTY_ASSIGNED_CONTEXT ( ( #7081 ) ) GLOBAL_UNIT_ASSIGNED_CONTEXT ( ( #23244, #17651, #15858 ) ) REPRESENTATION_CONTEXT ( 'NONE', 'WORKASPACE' ) );
#15319 = CARTESIAN_POINT ( 'NONE',  ( 17.33131581010000133, -22.98361965280000163, -147.5552959529999839 ) ) ;
#15320 = CARTESIAN_POINT ( 'NONE',  ( 31.00000000000000000, -39.80430157320000006, -151.0552959529999839 ) ) ;
#15321 = CARTESIAN_POINT ( 'NONE',  ( -9.870393330222821504, 37.85345449821588204, -147.8311166188136099 ) ) ;
#15322 = EDGE_LOOP ( 'NONE', ( #7584, #11020, #21763, #11408 ) ) ;
#15323 = CARTESIAN_POINT ( 'NONE',  ( 10.68320006080000084, -20.50000000000000000, -148.5552959529999839 ) ) ;
#15324 = CARTESIAN_POINT ( 'NONE',  ( 8.698426387723953823, 38.49992893826069462, -146.0553492493478132 ) ) ;
#15325 = CARTESIAN_POINT ( 'NONE',  ( 3.999999999879999546, -4.000000000000000000, -135.2552959529999725 ) ) ;
#15326 = VERTEX_POINT ( 'NONE', #4235 ) ;
#15327 = EDGE_CURVE ( 'NONE', #7397, #7104, #6488, .T. ) ;
#15328 = CARTESIAN_POINT ( 'NONE',  ( -18.18930989805799925, 36.96028804432503989, -147.6841622078449916 ) ) ;
#15329 = CARTESIAN_POINT ( 'NONE',  ( 1.133692148650000009, -50.50000000000000000, -136.0552959530000123 ) ) ;
#15330 = ORIENTED_EDGE ( 'NONE', *, *, #1239, .F. ) ;
#15331 = CARTESIAN_POINT ( 'NONE',  ( 6.500000000000000000, 28.00000000000000000, -151.0552959529999839 ) ) ;
#15332 = DIRECTION ( 'NONE',  ( 0.000000000000000000, -1.000000000000000000, 0.000000000000000000 ) ) ;
#15333 = ORIENTED_EDGE ( 'NONE', *, *, #10678, .T. ) ;
#15334 = CARTESIAN_POINT ( 'NONE',  ( 24.97526911139999939, 44.90215078659999648, -151.0552959529999839 ) ) ;
#15335 = CARTESIAN_POINT ( 'NONE',  ( 20.87864083493722234, -22.01085694111270641, -150.0552959530000123 ) ) ;
#15336 = ORIENTED_EDGE ( 'NONE', *, *, #3766, .F. ) ;
#15337 = VECTOR ( 'NONE', #14470, 1000.000000000000227 ) ;
#15338 = CARTESIAN_POINT ( 'NONE',  ( 6.499999999879999102, -4.000000000000000000, -135.2552959529999725 ) ) ;
#15339 = CARTESIAN_POINT ( 'NONE',  ( -25.61321927598924475, 33.33310017243326229, -146.2757612383772710 ) ) ;
#15340 = ORIENTED_EDGE ( 'NONE', *, *, #529, .F. ) ;
#15341 = EDGE_CURVE ( 'NONE', #4100, #22307, #7793, .T. ) ;
#15342 = CARTESIAN_POINT ( 'NONE',  ( 31.50000000000000000, 0.000000000000000000, -137.0552959530000123 ) ) ;
#15343 = ORIENTED_EDGE ( 'NONE', *, *, #10505, .F. ) ;
#15344 = CYLINDRICAL_SURFACE ( 'NONE', #2639, 9.999999999999998224 ) ;
#15345 = EDGE_CURVE ( 'NONE', #4350, #3167, #1404, .T. ) ;
#15346 = CARTESIAN_POINT ( 'NONE',  ( 17.06104532839999877, -32.02344838739999489, -143.0552959529999839 ) ) ;
#15347 = ORIENTED_EDGE ( 'NONE', *, *, #10821, .F. ) ;
#15348 = CARTESIAN_POINT ( 'NONE',  ( 31.00000000000000000, 39.80430157320000006, -150.0552959529999839 ) ) ;
#15349 = ADVANCED_FACE ( 'NONE', ( #17191 ), #10033, .T. ) ;
#15350 = ORIENTED_EDGE ( 'NONE', *, *, #14487, .T. ) ;
#15351 = CARTESIAN_POINT ( 'NONE',  ( -25.86630785139999844, -50.50000000000000000, -143.0552959529999839 ) ) ;
#15352 = EDGE_CURVE ( 'NONE', #20386, #22853, #602, .T. ) ;
#15353 = CARTESIAN_POINT ( 'NONE',  ( 1.600095057559999923, -18.40127899619999852, -145.5552959529999839 ) ) ;
#15354 = ORIENTED_EDGE ( 'NONE', *, *, #12736, .F. ) ;
#15355 = EDGE_LOOP ( 'NONE', ( #12703, #6364, #9446, #16734 ) ) ;
#15356 = CARTESIAN_POINT ( 'NONE',  ( 6.899000527194538712, -1.656359840075253942, -150.0552959529999839 ) ) ;
#15357 = CARTESIAN_POINT ( 'NONE',  ( -30.68396739435298670, 40.64794745105150753, -146.0701989576813844 ) ) ;
#15358 = DIRECTION ( 'NONE',  ( 1.000000000000000000, 0.000000000000000000, 0.000000000000000000 ) ) ;
#15359 = CARTESIAN_POINT ( 'NONE',  ( -20.60824191589624022, -3.803650459150011542, -146.3157682189980733 ) ) ;
#15360 = ORIENTED_EDGE ( 'NONE', *, *, #15793, .T. ) ;
#15361 = CARTESIAN_POINT ( 'NONE',  ( -16.49999999999998224, -42.80113973139842187, -136.0552959529627515 ) ) ;
#15362 = DIRECTION ( 'NONE',  ( -0.1809478134909354996, 0.9834926989016490317, 9.461363557886634012E-13 ) ) ;
#15363 = LINE ( 'NONE', #12016, #7509 ) ;
#15364 = DIRECTION ( 'NONE',  ( 0.000000000000000000, 1.000000000000000000, 0.000000000000000000 ) ) ;
#15365 = DIRECTION ( 'NONE',  ( 1.000000000000000000, 0.000000000000000000, -1.526556658859589738E-13 ) ) ;
#15366 = DIRECTION ( 'NONE',  ( -1.211690350420779919E-27, -2.765629237169220318E-27, 1.000000000000000000 ) ) ;
#15367 = EDGE_CURVE ( 'NONE', #11018, #21963, #16956, .T. ) ;
#15368 = CARTESIAN_POINT ( 'NONE',  ( -16.37184312240000139, 32.37338091950000063, -144.3414871020000021 ) ) ;
#15369 = EDGE_CURVE ( 'NONE', #14816, #8776, #20737, .T. ) ;
#15370 = LINE ( 'NONE', #626, #13359 ) ;
#15371 = DIRECTION ( 'NONE',  ( -0.9848077530125619594, 0.000000000000000000, -0.1736481776649230202 ) ) ;
#15372 = CARTESIAN_POINT ( 'NONE',  ( -6.547730170579999509, -18.66441632429999942, -147.5552959529999839 ) ) ;
#15373 = ORIENTED_EDGE ( 'NONE', *, *, #19713, .F. ) ;
#15374 = CARTESIAN_POINT ( 'NONE',  ( -10.75221293964388103, 33.20739279112564191, -143.4848104349948130 ) ) ;
#15375 = LINE ( 'NONE', #13111, #22149 ) ;
#15376 = DIRECTION ( 'NONE',  ( 1.000000000000000000, 0.000000000000000000, -2.262079412673756451E-12 ) ) ;
#15377 = ORIENTED_EDGE ( 'NONE', *, *, #21374, .F. ) ;
#15378 = CARTESIAN_POINT ( 'NONE',  ( 18.95053822279999878, -50.50000000000000000, -149.5552959529999839 ) ) ;
#15379 = CARTESIAN_POINT ( 'NONE',  ( -21.73453520643527881, 32.91403690840683538, -144.3663112597812130 ) ) ;
#15380 = DIRECTION ( 'NONE',  ( 4.430318231639999944E-12, -6.100259101500000139E-13, 1.000000000000000000 ) ) ;
#15381 = ORIENTED_EDGE ( 'NONE', *, *, #8799, .T. ) ;
#15382 = CARTESIAN_POINT ( 'NONE',  ( -22.73109880836567953, 38.77532135900968058, -140.2559096062584274 ) ) ;
#15383 = CARTESIAN_POINT ( 'NONE',  ( -9.334216945200001447, -17.19633444960000190, -146.5552959529999839 ) ) ;
#15384 = DIRECTION ( 'NONE',  ( 2.257144641399999941E-12, -4.009147065140000298E-51, 1.000000000000000000 ) ) ;
#15385 = CARTESIAN_POINT ( 'NONE',  ( -30.99999999989999822, 26.50000000000000000, -138.5552959529999839 ) ) ;
#15386 = CARTESIAN_POINT ( 'NONE',  ( -10.17933436543764003, 35.38122503070080427, -147.6311798951892058 ) ) ;
#15387 = CARTESIAN_POINT ( 'NONE',  ( -34.50000000000000000, 26.00000000000000000, -141.5552959529999839 ) ) ;
#15388 = CARTESIAN_POINT ( 'NONE',  ( -7.888511564689155264, 38.45496397857106530, -140.8398455980544099 ) ) ;
#15389 = ORIENTED_EDGE ( 'NONE', *, *, #17375, .T. ) ;
#15390 =( NAMED_UNIT ( * ) SI_UNIT ( $, .STERADIAN. ) SOLID_ANGLE_UNIT ( ) );
#15391 = ADVANCED_FACE ( 'NONE', ( #18859 ), #6360, .F. ) ;
#15392 = ADVANCED_FACE ( 'NONE', ( #2803 ), #22313, .F. ) ;
#15393 = ORIENTED_EDGE ( 'NONE', *, *, #3537, .F. ) ;
#15394 = CARTESIAN_POINT ( 'NONE',  ( -12.58047663530000015, 34.35960099889999952, -147.8017659109999897 ) ) ;
#15395 = CARTESIAN_POINT ( 'NONE',  ( 23.50000000000000000, -20.50000000000000000, -142.5552959529999839 ) ) ;
#15396 = CARTESIAN_POINT ( 'NONE',  ( 0.5000000001500000124, 24.10555127549999810, -143.5552959529999839 ) ) ;
#15397 =( BOUNDED_SURFACE ( )  B_SPLINE_SURFACE ( 5, 5, ( 
 ( #13036, #20306, #10279, #1146, #3042, #6594 ),
 ( #11821, #22909, #17189, #15649, #15521, #17550 ),
 ( #21007, #4698, #4345, #9914, #20889, #11579 ),
 ( #11939, #8376, #10030, #2917, #17306, #10149 ),
 ( #22552, #17422, #15404, #11698, #13857, #21125 ),
 ( #4578, #1268, #19330, #6243, #6357, #4816 ),
 ( #12059, #19095, #13492, #1020, #906, #8491 ),
 ( #18856, #19205, #15761, #23022, #6708, #13970 ),
 ( #2800, #2568, #9790, #17067, #18974, #788 ),
 ( #8014, #15297, #13613, #20766, #4459, #2687 ),
 ( #8247, #8132, #22783, #22662, #6483, #13742 ),
 ( #4936, #16117, #1372, #6830, #19922, #3621 ) ),
 .UNSPECIFIED., .F., .F., .F. ) 
 B_SPLINE_SURFACE_WITH_KNOTS ( ( 6, 3, 3, 6 ),
 ( 6, 6 ),
 ( 0.000000000000000000, 4.124045064660000648, 8.344666563069999654, 12.67057240369999960 ),
 ( 1.570796326600514936, 3.141592653590000062 ),
 .UNSPECIFIED. ) 
 GEOMETRIC_REPRESENTATION_ITEM ( )  RATIONAL_B_SPLINE_SURFACE ( (
 ( 0.2500000000000000000, 0.2499999999752375024, 0.2999999999628560343, 0.3999999999504744719, 0.5999999999504750381, 1.000000000000000000),
 ( 0.2500000000000000000, 0.2499999999752375024, 0.2999999999628560343, 0.3999999999504744719, 0.5999999999504750381, 1.000000000000000000),
 ( 0.2500000000000000000, 0.2499999999752375024, 0.2999999999628560343, 0.3999999999504744719, 0.5999999999504750381, 1.000000000000000000),
 ( 0.2500000000000000000, 0.2499999999752375024, 0.2999999999628560343, 0.3999999999504744719, 0.5999999999504750381, 1.000000000000000000),
 ( 0.2500000000000000000, 0.2499999999752375024, 0.2999999999628560343, 0.3999999999504744719, 0.5999999999504750381, 1.000000000000000000),
 ( 0.2500000000000000000, 0.2499999999752375024, 0.2999999999628560343, 0.3999999999504744719, 0.5999999999504750381, 1.000000000000000000),
 ( 0.2500000000000000000, 0.2499999999752375024, 0.2999999999628560343, 0.3999999999504744719, 0.5999999999504750381, 1.000000000000000000),
 ( 0.2500000000000000000, 0.2499999999752375024, 0.2999999999628560343, 0.3999999999504744719, 0.5999999999504750381, 1.000000000000000000),
 ( 0.2500000000000000000, 0.2499999999752375024, 0.2999999999628560343, 0.3999999999504744719, 0.5999999999504750381, 1.000000000000000000),
 ( 0.2500000000000000000, 0.2499999999752375024, 0.2999999999628560343, 0.3999999999504744719, 0.5999999999504750381, 1.000000000000000000),
 ( 0.2500000000000000000, 0.2499999999752375024, 0.2999999999628560343, 0.3999999999504744719, 0.5999999999504750381, 1.000000000000000000),
 ( 0.2500000000000000000, 0.2499999999752375024, 0.2999999999628560343, 0.3999999999504744719, 0.5999999999504750381, 1.000000000000000000) ) ) 
 REPRESENTATION_ITEM ( '' )  SURFACE ( )  );
#15398 = ORIENTED_EDGE ( 'NONE', *, *, #12164, .T. ) ;
#15399 = CARTESIAN_POINT ( 'NONE',  ( 8.500000000060001781, 38.50000000000000000, -142.0552959529999839 ) ) ;
#15400 = CARTESIAN_POINT ( 'NONE',  ( -14.45813593939999997, 41.09907220950000095, -141.6721478100000127 ) ) ;
#15401 = CIRCLE ( 'NONE', #22637, 2.000000000000000000 ) ;
#15402 = ORIENTED_EDGE ( 'NONE', *, *, #18049, .T. ) ;
#15403 = CARTESIAN_POINT ( 'NONE',  ( -21.35824191589999899, -32.00000000000000000, -146.2257682199999920 ) ) ;
#15404 = CARTESIAN_POINT ( 'NONE',  ( -18.01907198844549995, 40.17100866524817349, -142.0952484789442849 ) ) ;
#15405 = CARTESIAN_POINT ( 'NONE',  ( 7.510813698219587664, 38.13186516299664675, -146.2857056571632199 ) ) ;
#15406 = DIRECTION ( 'NONE',  ( -2.257144641399999941E-12, 0.000000000000000000, -1.000000000000000000 ) ) ;
#15407 = CARTESIAN_POINT ( 'NONE',  ( -24.20244548955877661, 34.61374440578268974, -147.2354883249831516 ) ) ;
#15408 = DIRECTION ( 'NONE',  ( 1.000000000000000000, 0.000000000000000000, 2.507771768020000122E-12 ) ) ;
#15409 = ORIENTED_EDGE ( 'NONE', *, *, #9531, .F. ) ;
#15410 = VECTOR ( 'NONE', #10316, 1000.000000000000227 ) ;
#15411 = DIRECTION ( 'NONE',  ( 1.000000000000000000, 2.004714280773594901E-17, -1.095180403012019938E-17 ) ) ;
#15412 = VECTOR ( 'NONE', #3163, 1000.000000000000000 ) ;
#15413 = ORIENTED_EDGE ( 'NONE', *, *, #18244, .T. ) ;
#15414 = CARTESIAN_POINT ( 'NONE',  ( -26.82473810827688254, 37.81866192723410336, -148.2916060357279378 ) ) ;
#15415 = ORIENTED_EDGE ( 'NONE', *, *, #9356, .T. ) ;
#15416 = EDGE_CURVE ( 'NONE', #6279, #7923, #21010, .T. ) ;
#15417 = CARTESIAN_POINT ( 'NONE',  ( 6.500000000170000014, 20.50000000000000000, -136.5552959530000123 ) ) ;
#15418 = ORIENTED_EDGE ( 'NONE', *, *, #23347, .T. ) ;
#15419 = FACE_OUTER_BOUND ( 'NONE', #12678, .T. ) ;
#15420 = ADVANCED_FACE ( 'NONE', ( #13260 ), #2460, .F. ) ;
#15421 = EDGE_LOOP ( 'NONE', ( #10266, #2062, #5816, #2404 ) ) ;
#15422 = ORIENTED_EDGE ( 'NONE', *, *, #17057, .F. ) ;
#15423 = FACE_OUTER_BOUND ( 'NONE', #19144, .T. ) ;
#15424 = CARTESIAN_POINT ( 'NONE',  ( -25.86630785129999666, -51.50000000000000000, -136.0552959530000123 ) ) ;
#15425 = CARTESIAN_POINT ( 'NONE',  ( -22.02741209360413777, -3.608510005928772468, -146.3157682189998070 ) ) ;
#15426 = CARTESIAN_POINT ( 'NONE',  ( -7.052957782236454420, 32.23883816114348377, -143.6422217563765287 ) ) ;
#15427 = CARTESIAN_POINT ( 'NONE',  ( 6.500000000030000002, 28.00000000000000000, -137.0552959530000123 ) ) ;
#15428 = ORIENTED_EDGE ( 'NONE', *, *, #2486, .F. ) ;
#15429 = DIRECTION ( 'NONE',  ( 0.000000000000000000, 1.000000000000000000, 2.257144641399999941E-12 ) ) ;
#15430 = VECTOR ( 'NONE', #8249, 1000.000000000000227 ) ;
#15431 = CIRCLE ( 'NONE', #5170, 7.000000000000000888 ) ;
#15432 = CARTESIAN_POINT ( 'NONE',  ( 8.892420295525585772, 38.46233185836359780, -146.0852624393696146 ) ) ;
#15433 = DIRECTION ( 'NONE',  ( -0.1435602414469281940, -0.9896415801065048257, 3.847089866708073804E-13 ) ) ;
#15434 = EDGE_LOOP ( 'NONE', ( #1027, #23312, #11060, #12724 ) ) ;
#15435 = PLANE ( 'NONE',  #21962 ) ;
#15436 = DIRECTION ( 'NONE',  ( 1.000000000000000000, -5.094701932209999624E-24, -2.257144641399999941E-12 ) ) ;
#15437 = EDGE_LOOP ( 'NONE', ( #12954, #3152, #15062, #18683 ) ) ;
#15438 = CARTESIAN_POINT ( 'NONE',  ( -12.50000000000000000, 48.50000000000000000, -137.0552959530000123 ) ) ;
#15439 = FACE_OUTER_BOUND ( 'NONE', #10677, .T. ) ;
#15440 = EDGE_LOOP ( 'NONE', ( #5002, #13835, #22833, #3438 ) ) ;
#15441 = DIRECTION ( 'NONE',  ( -1.000000000000000000, 0.000000000000000000, 0.000000000000000000 ) ) ;
#15442 = DIRECTION ( 'NONE',  ( -0.9753087663813413410, 0.2208456705930775810, 8.936242978303132921E-12 ) ) ;
#15443 = EDGE_LOOP ( 'NONE', ( #12294, #15540, #4063, #10348 ) ) ;
#15444 = CARTESIAN_POINT ( 'NONE',  ( -14.90221424347422818, 38.57597971860518982, -140.2753094542739802 ) ) ;
#15445 = AXIS2_PLACEMENT_3D ( 'NONE', #21071, #1213, #11886 ) ;
#15446 = CARTESIAN_POINT ( 'NONE',  ( -25.86608305657696860, 32.48195522393204016, -143.6651831558542369 ) ) ;
#15447 = EDGE_CURVE ( 'NONE', #19550, #8868, #399, .T. ) ;
#15448 = EDGE_LOOP ( 'NONE', ( #14507, #17897, #6500 ) ) ;
#15449 =( NAMED_UNIT ( * ) PLANE_ANGLE_UNIT ( ) SI_UNIT ( $, .RADIAN. ) );
#15450 = CARTESIAN_POINT ( 'NONE',  ( -33.50000000000000000, -1.000000000000000000, -140.0552959529999839 ) ) ;
#15451 = VERTEX_POINT ( 'NONE', #17070 ) ;
#15452 = LINE ( 'NONE', #17602, #14796 ) ;
#15453 = CARTESIAN_POINT ( 'NONE',  ( 3.999999999879999546, -4.000000000000000000, -135.4552959529999896 ) ) ;
#15454 = ORIENTED_EDGE ( 'NONE', *, *, #3080, .F. ) ;
#15455 = DIRECTION ( 'NONE',  ( 0.000000000000000000, -0.4794255386042033384, -0.8775825618903726477 ) ) ;
#15456 = PRODUCT_RELATED_PRODUCT_CATEGORY ( 'part', '', ( #10985 ) ) ;
#15457 = ORIENTED_EDGE ( 'NONE', *, *, #15126, .T. ) ;
#15458 = CARTESIAN_POINT ( 'NONE',  ( 1.600095057559999923, -18.40127899619999852, -146.5552959529999839 ) ) ;
#15459 = EDGE_CURVE ( 'NONE', #2337, #19493, #21369, .T. ) ;
#15460 = CARTESIAN_POINT ( 'NONE',  ( 4.499999999879999102, -3.500000000000000000, -139.0552959529999839 ) ) ;
#15461 = ORIENTED_EDGE ( 'NONE', *, *, #6933, .T. ) ;
#15462 = VECTOR ( 'NONE', #12351, 1000.000000000000000 ) ;
#15463 = ORIENTED_EDGE ( 'NONE', *, *, #5466, .F. ) ;
#15464 = DIRECTION ( 'NONE',  ( 0.000000000000000000, -1.000000000000000000, 0.000000000000000000 ) ) ;
#15465 = EDGE_CURVE ( 'NONE', #8748, #22265, #23019, .T. ) ;
#15466 = DIRECTION ( 'NONE',  ( 0.9985681355238719137, -0.05349466063429310358, -4.511742413209420161E-12 ) ) ;
#15467 = CARTESIAN_POINT ( 'NONE',  ( -22.10824191589999899, -32.00000000000000000, -145.5657682190000060 ) ) ;
#15468 = FACE_OUTER_BOUND ( 'NONE', #7568, .T. ) ;
#15469 = ORIENTED_EDGE ( 'NONE', *, *, #8827, .F. ) ;
#15470 = CARTESIAN_POINT ( 'NONE',  ( 10.68320006080000084, -19.50000000000000000, -150.0552959529999839 ) ) ;
#15471 = FACE_OUTER_BOUND ( 'NONE', #13673, .T. ) ;
#15472 = CARTESIAN_POINT ( 'NONE',  ( 26.42191803000494588, -19.71475634692216161, -150.0552959530000123 ) ) ;
#15473 = DIRECTION ( 'NONE',  ( -0.6459422414661291079, -0.7633862853691523176, -2.273736754430455399E-12 ) ) ;
#15474 = LINE ( 'NONE', #17622, #17920 ) ;
#15475 = CARTESIAN_POINT ( 'NONE',  ( 4.750000000030000002, -44.75000000000000000, -136.0552959530000123 ) ) ;
#15476 = ADVANCED_FACE ( 'NONE', ( #17907 ), #5059, .F. ) ;
#15477 = ORIENTED_EDGE ( 'NONE', *, *, #13860, .F. ) ;
#15478 = CARTESIAN_POINT ( 'NONE',  ( -16.36784392973273938, 33.86562477380443426, -142.0582287347409931 ) ) ;
#15479 = AXIS2_PLACEMENT_3D ( 'NONE', #21665, #20339, #2034 ) ;
#15480 = LINE ( 'NONE', #22738, #738 ) ;
#15481 = DIRECTION ( 'NONE',  ( 0.000000000000000000, 0.000000000000000000, 1.000000000000000000 ) ) ;
#15482 = CARTESIAN_POINT ( 'NONE',  ( 31.00000000000000000, -39.80430157320000006, -149.5552959529999839 ) ) ;
#15483 = CARTESIAN_POINT ( 'NONE',  ( -7.529689113779999943, 37.05876528330000497, -139.9906690790000141 ) ) ;
#15484 = ORIENTED_EDGE ( 'NONE', *, *, #9650, .T. ) ;
#15485 = CARTESIAN_POINT ( 'NONE',  ( -9.948438925625499252, 33.43836456409815838, -141.7026862686744835 ) ) ;
#15486 = PLANE ( 'NONE',  #5049 ) ;
#15487 = EDGE_CURVE ( 'NONE', #21810, #1162, #8933, .T. ) ;
#15488 = DIRECTION ( 'NONE',  ( -1.701177084980000217E-20, -4.426606872460000157E-37, -1.000000000000000000 ) ) ;
#15489 = VERTEX_POINT ( 'NONE', #15874 ) ;
#15490 = EDGE_CURVE ( 'NONE', #11102, #8120, #16120, .T. ) ;
#15491 = LINE ( 'NONE', #6568, #16754 ) ;
#15492 = FACE_OUTER_BOUND ( 'NONE', #563, .T. ) ;
#15493 = CARTESIAN_POINT ( 'NONE',  ( -9.347107914279998653, -17.32706600430000066, -143.5552959529999839 ) ) ;
#15494 = ORIENTED_EDGE ( 'NONE', *, *, #8183, .T. ) ;
#15495 = CARTESIAN_POINT ( 'NONE',  ( -23.40625992182578941, 38.40432287900232922, -140.8828493825280361 ) ) ;
#15496 = AXIS2_PLACEMENT_3D ( 'NONE', #14684, #5637, #5985 ) ;
#15497 = EDGE_CURVE ( 'NONE', #21310, #16420, #12302, .T. ) ;
#15498 = CYLINDRICAL_SURFACE ( 'NONE', #22267, 2.500000000000000444 ) ;
#15499 = EDGE_CURVE ( 'NONE', #23322, #19847, #14099, .T. ) ;
#15500 = CIRCLE ( 'NONE', #19290, 2.000000000000001776 ) ;
#15501 = CARTESIAN_POINT ( 'NONE',  ( -1.000000000000000000, 20.50000000000000000, -150.0552959529999839 ) ) ;
#15502 = LINE ( 'NONE', #20990, #3012 ) ;
#15503 = CARTESIAN_POINT ( 'NONE',  ( -9.971101149527340723, 37.05360750091212196, -147.8421425029205807 ) ) ;
#15504 = LINE ( 'NONE', #22764, #13888 ) ;
#15505 = EDGE_CURVE ( 'NONE', #17357, #21983, #23376, .T. ) ;
#15506 = CARTESIAN_POINT ( 'NONE',  ( 9.660841442678691493, -35.21298433615703516, -150.0552959529999839 ) ) ;
#15507 = PRODUCT ( 'Latch Bolt Assembly', 'Latch Bolt Assembly', '', ( #2019 ) ) ;
#15508 = EDGE_CURVE ( 'NONE', #1217, #1116, #6833, .T. ) ;
#15509 = ORIENTED_EDGE ( 'NONE', *, *, #22479, .T. ) ;
#15510 = FILL_AREA_STYLE ('',( #15747 ) ) ;
#15511 = EDGE_LOOP ( 'NONE', ( #22440, #2915, #326, #20325 ) ) ;
#15512 = CARTESIAN_POINT ( 'NONE',  ( -7.015833805750000707, 33.30032478630000270, -141.9582197170000200 ) ) ;
#15513 = CARTESIAN_POINT ( 'NONE',  ( -26.73151279740000064, 41.02465574069999121, -146.3859699699999908 ) ) ;
#15514 = CARTESIAN_POINT ( 'NONE',  ( -21.70878449369999785, 39.52018264390000013, -147.4849246469999855 ) ) ;
#15515 = VERTEX_POINT ( 'NONE', #19575 ) ;
#15516 = CARTESIAN_POINT ( 'NONE',  ( -15.46250806109999942, -34.50000000000000000, -147.7289441310000200 ) ) ;
#15517 = CARTESIAN_POINT ( 'NONE',  ( -15.47708384459999920, 37.95279615419999431, -148.5507537150000132 ) ) ;
#15518 = VECTOR ( 'NONE', #6603, 1000.000000000000000 ) ;
#15519 = EDGE_LOOP ( 'NONE', ( #16249, #22498, #1317, #11597 ) ) ;
#15520 = CARTESIAN_POINT ( 'NONE',  ( -20.84101097267440039, 38.55092845031688142, -147.7610021335696047 ) ) ;
#15521 = CARTESIAN_POINT ( 'NONE',  ( -17.62617954421223132, 37.82805002212005974, -139.7243320108600813 ) ) ;
#15522 = FACE_OUTER_BOUND ( 'NONE', #20293, .T. ) ;
#15523 = PLANE ( 'NONE',  #3795 ) ;
#15524 = CARTESIAN_POINT ( 'NONE',  ( 31.00000000000000000, -39.80430157320000006, -149.5552959529999839 ) ) ;
#15525 = EDGE_CURVE ( 'NONE', #8011, #22948, #13890, .T. ) ;
#15526 = CARTESIAN_POINT ( 'NONE',  ( -24.00819484748617327, 36.12951795105237096, -147.8708185612008208 ) ) ;
#15527 = CARTESIAN_POINT ( 'NONE',  ( 4.890616787569204149, -4.961649142147357416, -150.0552959529999839 ) ) ;
#15528 = AXIS2_PLACEMENT_3D ( 'NONE', #11969, #15551, #6737 ) ;
#15529 = VECTOR ( 'NONE', #9636, 1000.000000000000000 ) ;
#15530 = ORIENTED_EDGE ( 'NONE', *, *, #15670, .T. ) ;
#15531 = FACE_OUTER_BOUND ( 'NONE', #4297, .T. ) ;
#15532 = VECTOR ( 'NONE', #2158, 1000.000000000000000 ) ;
#15533 = ORIENTED_EDGE ( 'NONE', *, *, #8062, .T. ) ;
#15534 = SURFACE_STYLE_FILL_AREA ( #22324 ) ;
#15535 = ORIENTED_EDGE ( 'NONE', *, *, #12869, .T. ) ;
#15536 = VECTOR ( 'NONE', #14855, 1000.000000000000000 ) ;
#15537 = DIRECTION ( 'NONE',  ( -3.994014902950000436E-29, 1.000000000000000000, -4.148443855749999753E-27 ) ) ;
#15538 = VERTEX_POINT ( 'NONE', #21246 ) ;
#15539 = CARTESIAN_POINT ( 'NONE',  ( 3.175121949296230373, 27.24084097722929343, -136.0552959530071746 ) ) ;
#15540 = ORIENTED_EDGE ( 'NONE', *, *, #9513, .F. ) ;
#15541 = ORIENTED_EDGE ( 'NONE', *, *, #15155, .F. ) ;
#15542 = CARTESIAN_POINT ( 'NONE',  ( -12.00000000000000000, -43.00000000000000000, -145.5552959529999839 ) ) ;
#15543 = CARTESIAN_POINT ( 'NONE',  ( -18.90246017563120162, 37.04541408822156967, -147.4848489021858313 ) ) ;
#15544 = DIRECTION ( 'NONE',  ( 2.688820921349999492E-17, -1.000000000000000000, -6.069065783950000909E-29 ) ) ;
#15545 = LINE ( 'NONE', #20672, #7537 ) ;
#15546 = CARTESIAN_POINT ( 'NONE',  ( -7.296416894500538319, 32.72008036306245771, -141.6746418080609828 ) ) ;
#15547 = CIRCLE ( 'NONE', #16322, 0.5000000000000004441 ) ;
#15548 = CARTESIAN_POINT ( 'NONE',  ( -9.852708451402975243, 38.00872972452032883, -148.5766935762293031 ) ) ;
#15549 = ORIENTED_EDGE ( 'NONE', *, *, #737, .F. ) ;
#15550 = VECTOR ( 'NONE', #23231, 1000.000000000000000 ) ;
#15551 = DIRECTION ( 'NONE',  ( 8.955190032050000935E-12, -9.104778821549999739E-13, 1.000000000000000000 ) ) ;
#15552 = AXIS2_PLACEMENT_3D ( 'NONE', #1041, #22572, #13876 ) ;
#15553 = ADVANCED_FACE ( 'NONE', ( #3266 ), #14215, .F. ) ;
#15554 = CARTESIAN_POINT ( 'NONE',  ( -14.11967125440000004, 36.98834135279999913, -140.5455248810000057 ) ) ;
#15555 = VECTOR ( 'NONE', #1461, 1000.000000000000000 ) ;
#15556 = CARTESIAN_POINT ( 'NONE',  ( 8.250000000000000000, -40.23606797749999942, -151.0552959529999839 ) ) ;
#15557 = VERTEX_POINT ( 'NONE', #21482 ) ;
#15558 = DIRECTION ( 'NONE',  ( 1.000000000000000000, 0.000000000000000000, 2.516505522483685870E-12 ) ) ;
#15559 = DIRECTION ( 'NONE',  ( 2.257144641399999941E-12, 0.000000000000000000, 1.000000000000000000 ) ) ;
#15560 = VERTEX_POINT ( 'NONE', #12409 ) ;
#15561 = SURFACE_STYLE_FILL_AREA ( #8417 ) ;
#15562 = CARTESIAN_POINT ( 'NONE',  ( -6.683153925719999222, -50.50000000000000000, -149.5552959529999839 ) ) ;
#15563 = VECTOR ( 'NONE', #93, 1000.000000000000114 ) ;
#15564 = ORIENTED_EDGE ( 'NONE', *, *, #17873, .F. ) ;
#15565 = DIRECTION ( 'NONE',  ( 2.257157423930000049E-12, 0.000000000000000000, 1.000000000000000000 ) ) ;
#15566 = CARTESIAN_POINT ( 'NONE',  ( 25.01085694111271351, -23.12135916506276700, -150.0552959529999839 ) ) ;
#15567 = ORIENTED_EDGE ( 'NONE', *, *, #18394, .T. ) ;
#15568 = FACE_OUTER_BOUND ( 'NONE', #12226, .T. ) ;
#15569 = VECTOR ( 'NONE', #17615, 1000.000000000000227 ) ;
#15570 = CARTESIAN_POINT ( 'NONE',  ( -26.01424353331992734, 34.14238437626309519, -140.2248994934187181 ) ) ;
#15571 = EDGE_LOOP ( 'NONE', ( #7535, #13203, #4275, #2765 ) ) ;
#15572 = VECTOR ( 'NONE', #4363, 1000.000000000000000 ) ;
#15573 = VECTOR ( 'NONE', #19113, 1000.000000000000000 ) ;
#15574 = DIRECTION ( 'NONE',  ( 0.000000000000000000, 1.000000000000000000, 0.000000000000000000 ) ) ;
#15575 = ORIENTED_EDGE ( 'NONE', *, *, #7618, .F. ) ;
#15576 = VECTOR ( 'NONE', #15441, 1000.000000000000000 ) ;
#15577 = CARTESIAN_POINT ( 'NONE',  ( -2.499999999949999996, 32.75000000000000000, -150.0552959529999839 ) ) ;
#15578 = B_SPLINE_CURVE_WITH_KNOTS ( 'NONE', 1,
 ( #6739, #11972 ),
 .UNSPECIFIED., .F., .F.,
 ( 2, 2 ),
 ( -8.099639781629999646, 8.099639781629999646 ),
 .UNSPECIFIED. ) ;
#15579 = PLANE ( 'NONE',  #7318 ) ;
#15580 = ORIENTED_EDGE ( 'NONE', *, *, #11966, .T. ) ;
#15581 = CARTESIAN_POINT ( 'NONE',  ( -21.35824191589999899, -32.00000000000000000, -144.8157682190000060 ) ) ;
#15582 = ORIENTED_EDGE ( 'NONE', *, *, #12324, .T. ) ;
#15583 = LINE ( 'NONE', #14030, #17816 ) ;
#15584 = CARTESIAN_POINT ( 'NONE',  ( -24.57863953949999924, 33.12365565980000071, -146.2648171790000049 ) ) ;
#15585 = VERTEX_POINT ( 'NONE', #10153 ) ;
#15586 = EDGE_CURVE ( 'NONE', #22593, #20530, #4702, .T. ) ;
#15587 = EDGE_CURVE ( 'NONE', #7890, #17719, #19209, .T. ) ;
#15588 = ORIENTED_EDGE ( 'NONE', *, *, #1037, .T. ) ;
#15589 = VECTOR ( 'NONE', #11574, 1000.000000000000227 ) ;
#15590 = VECTOR ( 'NONE', #18496, 1000.000000000000000 ) ;
#15591 = CARTESIAN_POINT ( 'NONE',  ( 8.982728679470000088, -17.28848751049999777, -144.0552959529999839 ) ) ;
#15592 = CARTESIAN_POINT ( 'NONE',  ( -21.63220705389140619, 37.01315499805642162, -148.7192284428339804 ) ) ;
#15593 = VECTOR ( 'NONE', #5175, 1000.000000000000000 ) ;
#15594 = CARTESIAN_POINT ( 'NONE',  ( -14.47497890702397605, 41.61557973986633385, -144.5624617423342784 ) ) ;
#15595 = PLANE ( 'NONE',  #19362 ) ;
#15596 = EDGE_LOOP ( 'NONE', ( #15701, #15887, #6233, #9219 ) ) ;
#15597 = DIRECTION ( 'NONE',  ( -1.000000000000000000, 0.000000000000000000, 0.000000000000000000 ) ) ;
#15598 = CARTESIAN_POINT ( 'NONE',  ( 19.91945158500000090, 51.14507942810000429, -149.8052959529999839 ) ) ;
#15599 = CARTESIAN_POINT ( 'NONE',  ( 32.50000000000000000, -21.03620104879999886, -136.5552959530000123 ) ) ;
#15600 = CARTESIAN_POINT ( 'NONE',  ( -15.75716798047311862, -41.69030790613991400, -150.0552959529999555 ) ) ;
#15601 = CARTESIAN_POINT ( 'NONE',  ( 5.792747474889999637, -16.92794981449999980, -144.5552959529999839 ) ) ;
#15602 = DIRECTION ( 'NONE',  ( 0.7071067811866730279, -0.3390050494208429743, -0.6205445805637129775 ) ) ;
#15603 = ORIENTED_EDGE ( 'NONE', *, *, #20145, .F. ) ;
#15604 = LINE ( 'NONE', #19414, #16778 ) ;
#15605 = LINE ( 'NONE', #1452, #18214 ) ;
#15606 = DIRECTION ( 'NONE',  ( -0.9892101392001055871, 0.1465035852930155202, 0.000000000000000000 ) ) ;
#15607 = DIRECTION ( 'NONE',  ( 0.000000000000000000, 0.000000000000000000, 1.000000000000000000 ) ) ;
#15608 = DIRECTION ( 'NONE',  ( 0.9996028016287901163, -0.02818224575639410520, -1.295785648389728035E-13 ) ) ;
#15609 = VECTOR ( 'NONE', #20065, 999.9999999999998863 ) ;
#15610 = EDGE_CURVE ( 'NONE', #9566, #20428, #8384, .T. ) ;
#15611 = ORIENTED_EDGE ( 'NONE', *, *, #16368, .T. ) ;
#15612 = DIRECTION ( 'NONE',  ( 1.000000000000000000, 0.000000000000000000, 0.000000000000000000 ) ) ;
#15613 = CYLINDRICAL_SURFACE ( 'NONE', #500, 7.500000000000006217 ) ;
#15614 = CARTESIAN_POINT ( 'NONE',  ( 3.742832019563417045, -2.190307906135578797, -150.0552959529999839 ) ) ;
#15615 = ORIENTED_EDGE ( 'NONE', *, *, #12298, .F. ) ;
#15616 = PRODUCT_DEFINITION_SHAPE ( 'NONE', 'NONE',  #1805 ) ;
#15617 = CARTESIAN_POINT ( 'NONE',  ( -37.07045745269999770, 47.50000000000000000, -139.0687076600000012 ) ) ;
#15618 = DIRECTION ( 'NONE',  ( 0.000000000000000000, -1.000000000000000000, 0.000000000000000000 ) ) ;
#15619 = EDGE_CURVE ( 'NONE', #3677, #12862, #21128, .T. ) ;
#15620 = FACE_OUTER_BOUND ( 'NONE', #1390, .T. ) ;
#15621 = ORIENTED_EDGE ( 'NONE', *, *, #12729, .F. ) ;
#15622 = CARTESIAN_POINT ( 'NONE',  ( -23.81889237380000068, 39.38287674749999923, -140.7489234159999967 ) ) ;
#15623 = DIRECTION ( 'NONE',  ( -1.000000000000000000, 0.000000000000000000, 2.273736754430000208E-12 ) ) ;
#15624 = CARTESIAN_POINT ( 'NONE',  ( -13.86630785130000021, -51.50000000000000000, -136.5552959530000123 ) ) ;
#15625 = CARTESIAN_POINT ( 'NONE',  ( 32.50000000000000000, 39.80430157340000363, -150.0552959529999839 ) ) ;
#15626 = DIRECTION ( 'NONE',  ( 0.000000000000000000, 0.000000000000000000, -1.000000000000000000 ) ) ;
#15627 = VECTOR ( 'NONE', #14007, 1000.000000000000000 ) ;
#15628 = CARTESIAN_POINT ( 'NONE',  ( 6.500000000000000000, 28.00000000000000000, -150.0552959529999839 ) ) ;
#15629 = PRESENTATION_LAYER_ASSIGNMENT (  '', '', ( #21327 ) ) ;
#15630 = CARTESIAN_POINT ( 'NONE',  ( 3.775218130398811045, -35.50714246577857836, -150.0552959529999555 ) ) ;
#15631 = EDGE_CURVE ( 'NONE', #22408, #15229, #19084, .T. ) ;
#15632 = ORIENTED_EDGE ( 'NONE', *, *, #3210, .T. ) ;
#15633 = DIRECTION ( 'NONE',  ( 1.000000000000000000, 0.000000000000000000, 0.000000000000000000 ) ) ;
#15634 = VERTEX_POINT ( 'NONE', #12186 ) ;
#15635 = CARTESIAN_POINT ( 'NONE',  ( -6.131111726649999483, 36.14321585209999910, -147.9535578170000178 ) ) ;
#15636 = CARTESIAN_POINT ( 'NONE',  ( -21.35824191591069265, -4.000000000000000000, -141.9623572383524959 ) ) ;
#15637 = CARTESIAN_POINT ( 'NONE',  ( 16.16922456049999823, -22.27514461170000004, -148.5552959529999839 ) ) ;
#15638 = EDGE_CURVE ( 'NONE', #11545, #760, #19462, .T. ) ;
#15639 = ORIENTED_EDGE ( 'NONE', *, *, #19756, .F. ) ;
#15640 = CARTESIAN_POINT ( 'NONE',  ( -31.00000000000000000, -51.00000000000000000, -149.5552959529999839 ) ) ;
#15641 = FACE_OUTER_BOUND ( 'NONE', #5384, .T. ) ;
#15642 = EDGE_CURVE ( 'NONE', #467, #23250, #10980, .T. ) ;
#15643 = AXIS2_PLACEMENT_3D ( 'NONE', #9747, #20264, #9524 ) ;
#15644 = ORIENTED_EDGE ( 'NONE', *, *, #3505, .F. ) ;
#15645 = VECTOR ( 'NONE', #14111, 1000.000000000000000 ) ;
#15646 = DIRECTION ( 'NONE',  ( 1.000000000000000000, 0.000000000000000000, 2.516505522483685870E-12 ) ) ;
#15647 = ADVANCED_FACE ( 'NONE', ( #7186 ), #14453, .T. ) ;
#15648 = EDGE_CURVE ( 'NONE', #9722, #2716, #12889, .T. ) ;
#15649 = CARTESIAN_POINT ( 'NONE',  ( -17.78798770263510320, 37.73719101445376367, -140.0682257265029023 ) ) ;
#15650 = CARTESIAN_POINT ( 'NONE',  ( 31.82297112100000192, -40.41789419119999849, -136.0552959530000123 ) ) ;
#15651 = B_SPLINE_CURVE_WITH_KNOTS ( 'NONE', 3,
 ( #20821, #10211, #2747, #8435 ),
 .UNSPECIFIED., .F., .F.,
 ( 4, 4 ),
 ( 0.000000000000000000, 0.8059436278830001132 ),
 .UNSPECIFIED. ) ;
#15652 = CARTESIAN_POINT ( 'NONE',  ( 7.370503126277467842, 36.00792309428232585, -146.3513483205678369 ) ) ;
#15653 = CARTESIAN_POINT ( 'NONE',  ( 4.499999999879999102, -3.500000000000000000, -135.0552959530000123 ) ) ;
#15654 = CARTESIAN_POINT ( 'NONE',  ( -24.84704225925436916, 37.03879906168187830, -147.5513581853046219 ) ) ;
#15655 = DIRECTION ( 'NONE',  ( 1.526468026909924924E-13, 8.159623473500010254E-13, 1.000000000000000000 ) ) ;
#15656 = DIRECTION ( 'NONE',  ( 2.257157423930000049E-12, 0.000000000000000000, 1.000000000000000000 ) ) ;
#15657 = ORIENTED_EDGE ( 'NONE', *, *, #6232, .T. ) ;
#15658 = LINE ( 'NONE', #19103, #21612 ) ;
#15659 = AXIS2_PLACEMENT_3D ( 'NONE', #9578, #22211, #20205 ) ;
#15660 = AXIS2_PLACEMENT_3D ( 'NONE', #15636, #19320, #10021 ) ;
#15661 = EDGE_CURVE ( 'NONE', #5099, #7733, #3973, .T. ) ;
#15662 = AXIS2_PLACEMENT_3D ( 'NONE', #14930, #897, #20757 ) ;
#15663 = ORIENTED_EDGE ( 'NONE', *, *, #17430, .T. ) ;
#15664 = VERTEX_POINT ( 'NONE', #5633 ) ;
#15665 = FACE_OUTER_BOUND ( 'NONE', #10002, .T. ) ;
#15666 = ORIENTED_EDGE ( 'NONE', *, *, #18272, .T. ) ;
#15667 = CARTESIAN_POINT ( 'NONE',  ( 19.13369214879999802, -50.49999999980000354, -143.0552959529999839 ) ) ;
#15668 = CARTESIAN_POINT ( 'NONE',  ( 29.68320006080000084, -24.50000000000000000, -148.5552959529999839 ) ) ;
#15669 = ORIENTED_EDGE ( 'NONE', *, *, #11384, .F. ) ;
#15670 = EDGE_CURVE ( 'NONE', #20191, #2000, #9303, .T. ) ;
#15671 = EDGE_LOOP ( 'NONE', ( #3787, #8594, #21270, #11332 ) ) ;
#15672 = CARTESIAN_POINT ( 'NONE',  ( -32.50000000000000000, 10.25000000050000004, -137.0552959530000123 ) ) ;
#15673 = CARTESIAN_POINT ( 'NONE',  ( -18.46643761637815828, 34.84883242728916031, -147.1252693408089840 ) ) ;
#15674 = ADVANCED_FACE ( 'NONE', ( #20169 ), #5412, .F. ) ;
#15675 = CARTESIAN_POINT ( 'NONE',  ( 2.499999999879999990, -3.500000000000000000, -143.0552959529999839 ) ) ;
#15676 = CARTESIAN_POINT ( 'NONE',  ( -9.282104535849999394, -16.71402168319999859, -144.5552959529999839 ) ) ;
#15677 = CARTESIAN_POINT ( 'NONE',  ( -6.481896728065510871, 33.11542685677439124, -146.3378416582211230 ) ) ;
#15678 = CARTESIAN_POINT ( 'NONE',  ( -10.14042191033886020, 37.07381867794361341, -148.2039739395295612 ) ) ;
#15679 = VERTEX_POINT ( 'NONE', #8958 ) ;
#15680 = DIRECTION ( 'NONE',  ( 1.000000000000000000, 0.000000000000000000, -4.510774274160000731E-12 ) ) ;
#15681 = VECTOR ( 'NONE', #21179, 1000.000000000000000 ) ;
#15682 = CARTESIAN_POINT ( 'NONE',  ( 23.28059818845795803, 33.57621958799324347, -150.0552959530000123 ) ) ;
#15683 = VERTEX_POINT ( 'NONE', #11206 ) ;
#15684 = LINE ( 'NONE', #4733, #22715 ) ;
#15685 = CARTESIAN_POINT ( 'NONE',  ( 25.00000000000000000, -20.50000000000000000, -136.0552959530000123 ) ) ;
#15686 = ORIENTED_EDGE ( 'NONE', *, *, #17667, .F. ) ;
#15687 = LINE ( 'NONE', #11979, #1079 ) ;
#15688 = CARTESIAN_POINT ( 'NONE',  ( 31.50000000000000000, -33.03620104880000241, -137.0552959530000123 ) ) ;
#15689 = ORIENTED_EDGE ( 'NONE', *, *, #9657, .T. ) ;
#15690 = DIRECTION ( 'NONE',  ( 1.000000000000000000, 0.000000000000000000, -2.257171095940000041E-12 ) ) ;
#15691 = LINE ( 'NONE', #4624, #862 ) ;
#15692 = ORIENTED_EDGE ( 'NONE', *, *, #10611, .F. ) ;
#15693 = CARTESIAN_POINT ( 'NONE',  ( -14.83278250954328037, 40.60058613834879537, -144.4189779530036049 ) ) ;
#15694 = CARTESIAN_POINT ( 'NONE',  ( -26.41286337068730461, 35.11800629833786047, -140.0118796628326834 ) ) ;
#15695 = VERTEX_POINT ( 'NONE', #1972 ) ;
#15696 = VECTOR ( 'NONE', #21502, 1000.000000000000000 ) ;
#15697 = EDGE_CURVE ( 'NONE', #2813, #15749, #16240, .T. ) ;
#15698 = ORIENTED_EDGE ( 'NONE', *, *, #14751, .T. ) ;
#15699 = DIRECTION ( 'NONE',  ( 0.000000000000000000, 0.000000000000000000, 1.000000000000000000 ) ) ;
#15700 = DIRECTION ( 'NONE',  ( 4.430233957459999899E-12, -6.092903959140000514E-13, 1.000000000000000000 ) ) ;
#15701 = ORIENTED_EDGE ( 'NONE', *, *, #7122, .F. ) ;
#15702 = DIRECTION ( 'NONE',  ( -2.507771768019999718E-12, -1.592654864209999947E-17, 1.000000000000000000 ) ) ;
#15703 = CARTESIAN_POINT ( 'NONE',  ( 14.00000000000000000, 20.50000000000000000, -150.0552959529999839 ) ) ;
#15704 = CARTESIAN_POINT ( 'NONE',  ( -1.499999999959999553, 44.76558107705088929, -136.0552959529966301 ) ) ;
#15705 =( GEOMETRIC_REPRESENTATION_CONTEXT ( 3 ) GLOBAL_UNCERTAINTY_ASSIGNED_CONTEXT ( ( #182 ) ) GLOBAL_UNIT_ASSIGNED_CONTEXT ( ( #19737, #14146, #15920 ) ) REPRESENTATION_CONTEXT ( 'NONE', 'WORKASPACE' ) );
#15706 = ORIENTED_EDGE ( 'NONE', *, *, #16527, .F. ) ;
#15707 = DIRECTION ( 'NONE',  ( 2.257144641397284947E-12, 2.714590281723094849E-24, 1.000000000000000000 ) ) ;
#15708 = CARTESIAN_POINT ( 'NONE',  ( 17.21087225569999646, -22.66053313549999970, -144.5552959529999839 ) ) ;
#15709 = CARTESIAN_POINT ( 'NONE',  ( -15.27002291898349995, 38.46844526377720541, -147.3668459616200153 ) ) ;
#15710 = LINE ( 'NONE', #19159, #2290 ) ;
#15711 = VERTEX_POINT ( 'NONE', #16695 ) ;
#15712 = CARTESIAN_POINT ( 'NONE',  ( 10.68320006080000084, -20.50000000000000000, -148.5552959529999839 ) ) ;
#15713 = CARTESIAN_POINT ( 'NONE',  ( -4.499999999939999995, 37.00000000000000000, -144.0552959529999839 ) ) ;
#15714 = CARTESIAN_POINT ( 'NONE',  ( 20.50000000000000000, -20.50000000000000000, -150.0552959529999839 ) ) ;
#15715 = LINE ( 'NONE', #22977, #381 ) ;
#15716 = DIRECTION ( 'NONE',  ( 1.000000000000000000, 0.000000000000000000, 2.516505522483685870E-12 ) ) ;
#15717 = CYLINDRICAL_SURFACE ( 'NONE', #719, 2.000000000000007994 ) ;
#15718 = ORIENTED_EDGE ( 'NONE', *, *, #7493, .F. ) ;
#15719 = CARTESIAN_POINT ( 'NONE',  ( -15.86130022171997389, 33.41189223525291396, -141.7054377170709927 ) ) ;
#15720 = ADVANCED_FACE ( 'NONE', ( #12532 ), #10742, .F. ) ;
#15721 = CARTESIAN_POINT ( 'NONE',  ( 25.50000000000000000, 19.50000000000000000, -150.0552959529999839 ) ) ;
#15722 = CARTESIAN_POINT ( 'NONE',  ( 25.50000000000000000, -2.273736754430000208E-12, -136.0552959530000123 ) ) ;
#15723 = FACE_OUTER_BOUND ( 'NONE', #8903, .T. ) ;
#15724 = EDGE_CURVE ( 'NONE', #4735, #1301, #20280, .T. ) ;
#15725 = CARTESIAN_POINT ( 'NONE',  ( 5.631397321050000571, -17.85059010000000157, -146.5552959529999839 ) ) ;
#15726 = VERTEX_POINT ( 'NONE', #19814 ) ;
#15727 = CARTESIAN_POINT ( 'NONE',  ( -10.56415788819999868, 36.18163687389999694, -139.7056672729999889 ) ) ;
#15728 = VECTOR ( 'NONE', #21058, 1000.000000000000000 ) ;
#15729 = DIRECTION ( 'NONE',  ( -2.257171095940000041E-12, 7.494005416210000121E-16, -1.000000000000000000 ) ) ;
#15730 = DIRECTION ( 'NONE',  ( 1.000000000000000000, 0.000000000000000000, 0.000000000000000000 ) ) ;
#15731 = EDGE_LOOP ( 'NONE', ( #7033, #10026, #4153, #23386 ) ) ;
#15732 = CARTESIAN_POINT ( 'NONE',  ( -29.03767587600000155, 36.26045984259999955, -140.5446710220000170 ) ) ;
#15733 = CARTESIAN_POINT ( 'NONE',  ( 8.500000000050000892, 37.00000000000000000, -149.5552959529999839 ) ) ;
#15734 = EDGE_LOOP ( 'NONE', ( #8709, #23315, #3032 ) ) ;
#15735 = CARTESIAN_POINT ( 'NONE',  ( -23.90246201272782400, 40.41935502004460545, -144.4616775445051644 ) ) ;
#15736 = DIRECTION ( 'NONE',  ( 1.000000000000000000, -5.094701932209999624E-24, 0.000000000000000000 ) ) ;
#15737 = CARTESIAN_POINT ( 'NONE',  ( 22.37638267690557115, -15.34326802965495773, -144.5552959530006945 ) ) ;
#15738 = CARTESIAN_POINT ( 'NONE',  ( 8.155284681625030174, 38.46058812810072425, -142.0263608015445982 ) ) ;
#15739 = ORIENTED_EDGE ( 'NONE', *, *, #16819, .F. ) ;
#15740 = CARTESIAN_POINT ( 'NONE',  ( 6.500000000140000012, 20.50000000000000000, -146.5552959529999839 ) ) ;
#15741 = FACE_OUTER_BOUND ( 'NONE', #5783, .T. ) ;
#15742 = CARTESIAN_POINT ( 'NONE',  ( 8.920566648557704426, -33.90725470905313443, -150.0552959529999839 ) ) ;
#15743 = DIRECTION ( 'NONE',  ( 0.000000000000000000, 0.000000000000000000, -1.000000000000000000 ) ) ;
#15744 = AXIS2_PLACEMENT_3D ( 'NONE', #16711, #7885, #14932 ) ;
#15745 = ORIENTED_EDGE ( 'NONE', *, *, #11707, .T. ) ;
#15746 = SHAPE_REPRESENTATION ( 'Lock Tumblers', ( #5025 ), #13402 ) ;
#15747 = FILL_AREA_STYLE_COLOUR ( '', #3468 ) ;
#15748 =( LENGTH_UNIT ( ) NAMED_UNIT ( * ) SI_UNIT ( .MILLI., .METRE. ) );
#15749 = VERTEX_POINT ( 'NONE', #287 ) ;
#15750 = CARTESIAN_POINT ( 'NONE',  ( -6.993473002926046789, 35.65312348993318636, -147.2648311488452748 ) ) ;
#15751 = CARTESIAN_POINT ( 'NONE',  ( -26.16983372440000011, 40.98399646770000260, -141.7700373849999949 ) ) ;
#15752 = ADVANCED_FACE ( 'NONE', ( #12657 ), #19925, .T. ) ;
#15753 = CARTESIAN_POINT ( 'NONE',  ( -22.00705883600000234, 37.05789963359999462, -148.1619053240000028 ) ) ;
#15754 = B_SPLINE_CURVE_WITH_KNOTS ( 'NONE', 3,
 ( #3643, #12430, #18156, #16376, #10758, #21856, #14588, #7209, #23157, #6851, #21387, #14472, #14347, #1518, #5073, #12317, #19592, #3285 ),
 .UNSPECIFIED., .F., .F.,
 ( 4, 2, 2, 2, 2, 2, 2, 2, 4 ),
 ( 0.000000000000000000, 0.1250000000000000000, 0.2500000000000000000, 0.3750000000000000000, 0.5000000000000000000, 0.6250000000000000000, 0.7500000000000000000, 0.8750000000000000000, 1.000000000000000000 ),
 .UNSPECIFIED. ) ;
#15755 = ORIENTED_EDGE ( 'NONE', *, *, #13561, .T. ) ;
#15756 = DIRECTION ( 'NONE',  ( 1.000000000000000000, 0.000000000000000000, -2.262079412673756451E-12 ) ) ;
#15757 = CARTESIAN_POINT ( 'NONE',  ( 6.000000000160000013, 29.48610037779999971, -140.5552959529999839 ) ) ;
#15758 = ORIENTED_EDGE ( 'NONE', *, *, #11609, .F. ) ;
#15759 = CARTESIAN_POINT ( 'NONE',  ( -21.35824191589999899, -4.000000000000000000, -144.8157682190000060 ) ) ;
#15760 = EDGE_CURVE ( 'NONE', #22442, #4332, #18481, .T. ) ;
#15761 = CARTESIAN_POINT ( 'NONE',  ( -18.43821035757416027, 40.21414801953198292, -145.7948256318368578 ) ) ;
#15762 = LINE ( 'NONE', #15650, #22665 ) ;
#15763 = CARTESIAN_POINT ( 'NONE',  ( 5.523675324947334708, -46.35111558253264263, -136.0552959530124610 ) ) ;
#15764 = CARTESIAN_POINT ( 'NONE',  ( -6.804059094464555812, 37.03366832433020761, -147.4295713063915230 ) ) ;
#15765 = DIRECTION ( 'NONE',  ( 1.000000000000000000, 0.000000000000000000, -4.430318231639999944E-12 ) ) ;
#15766 = PLANE ( 'NONE',  #3686 ) ;
#15767 = CARTESIAN_POINT ( 'NONE',  ( 2.218297500549999857, -15.44723318490000175, -147.0552959529999839 ) ) ;
#15768 = EDGE_CURVE ( 'NONE', #19021, #15273, #13010, .T. ) ;
#15769 = EDGE_LOOP ( 'NONE', ( #9653, #18760, #9950, #13831 ) ) ;
#15770 = DIRECTION ( 'NONE',  ( 0.000000000000000000, -1.000000000000000000, 1.723073263340000007E-12 ) ) ;
#15771 = ADVANCED_FACE ( 'NONE', ( #18022 ), #7418, .T. ) ;
#15772 = ORIENTED_EDGE ( 'NONE', *, *, #9731, .F. ) ;
#15773 = FILL_AREA_STYLE_COLOUR ( '', #19068 ) ;
#15774 = ORIENTED_EDGE ( 'NONE', *, *, #22460, .T. ) ;
#15775 = VECTOR ( 'NONE', #4760, 1000.000000000000000 ) ;
#15776 = CARTESIAN_POINT ( 'NONE',  ( -5.758148842630000708, -13.22138763369999914, -147.5552959529999839 ) ) ;
#15777 = CARTESIAN_POINT ( 'NONE',  ( -28.52142019845012655, 37.05975231236342182, -139.6605181375830682 ) ) ;
#15778 = ORIENTED_EDGE ( 'NONE', *, *, #6869, .T. ) ;
#15779 = VERTEX_POINT ( 'NONE', #16357 ) ;
#15780 = CARTESIAN_POINT ( 'NONE',  ( -16.81794493339999619, 37.02435727940000731, -140.5111119820000170 ) ) ;
#15781 = CARTESIAN_POINT ( 'NONE',  ( 31.50000000000000000, 20.96379895120000114, -143.0552959529999839 ) ) ;
#15782 = CARTESIAN_POINT ( 'NONE',  ( -11.68420994734520235, 39.25205177024059822, -141.0178453344531988 ) ) ;
#15783 = CARTESIAN_POINT ( 'NONE',  ( 29.68320006080000084, -7.750000000000000000, -150.0552959529999839 ) ) ;
#15784 = ORIENTED_EDGE ( 'NONE', *, *, #10078, .F. ) ;
#15785 = EDGE_CURVE ( 'NONE', #1140, #9187, #64, .T. ) ;
#15786 = CARTESIAN_POINT ( 'NONE',  ( 1.807537990517430693, -16.33773399031227314, -145.5552959529913437 ) ) ;
#15787 = EDGE_CURVE ( 'NONE', #6748, #7133, #20043, .T. ) ;
#15788 = CARTESIAN_POINT ( 'NONE',  ( 4.892621826548920083, -4.960959015002474715, -136.0552959530008934 ) ) ;
#15789 = VECTOR ( 'NONE', #22508, 1000.000000000000114 ) ;
#15790 = FACE_OUTER_BOUND ( 'NONE', #8535, .T. ) ;
#15791 = VECTOR ( 'NONE', #23026, 1000.000000000000000 ) ;
#15792 = EDGE_LOOP ( 'NONE', ( #20278, #23445, #15970, #4784 ) ) ;
#15793 = EDGE_CURVE ( 'NONE', #2929, #21873, #5980, .T. ) ;
#15794 = EDGE_CURVE ( 'NONE', #2684, #22598, #4436, .T. ) ;
#15795 = CARTESIAN_POINT ( 'NONE',  ( -32.50000000000000000, 65.58229784559999587, -147.5656262009999864 ) ) ;
#15796 = ORIENTED_EDGE ( 'NONE', *, *, #8750, .F. ) ;
#15797 = DIRECTION ( 'NONE',  ( 2.257171095940000041E-12, 1.003664318210000046E-28, 1.000000000000000000 ) ) ;
#15798 = LINE ( 'NONE', #23062, #8569 ) ;
#15799 = EDGE_CURVE ( 'NONE', #15020, #2120, #17043, .T. ) ;
#15800 = ORIENTED_EDGE ( 'NONE', *, *, #14481, .T. ) ;
#15801 = LINE ( 'NONE', #8420, #19368 ) ;
#15802 = DIRECTION ( 'NONE',  ( 1.000000000000000000, 2.602084704489999637E-17, -1.701177084980000217E-20 ) ) ;
#15803 = EDGE_LOOP ( 'NONE', ( #2347, #4368, #9811, #21848 ) ) ;
#15804 = CARTESIAN_POINT ( 'NONE',  ( -34.50000000000000000, -64.50000000000000000, -144.0552959529999839 ) ) ;
#15805 = CARTESIAN_POINT ( 'NONE',  ( -26.19803085470000070, 35.41001212129999942, -140.6029839040000127 ) ) ;
#15806 = ORIENTED_EDGE ( 'NONE', *, *, #3400, .F. ) ;
#15807 = FILL_AREA_STYLE ('',( #6642 ) ) ;
#15808 = ORIENTED_EDGE ( 'NONE', *, *, #13438, .T. ) ;
#15809 = AXIS2_PLACEMENT_3D ( 'NONE', #1303, #1058, #6867 ) ;
#15810 = CARTESIAN_POINT ( 'NONE',  ( -0.6781431574050000854, -62.17334590100000469, -148.0552959529999839 ) ) ;
#15811 = VERTEX_POINT ( 'NONE', #8110 ) ;
#15812 = VECTOR ( 'NONE', #3833, 1000.000000000000000 ) ;
#15813 = CARTESIAN_POINT ( 'NONE',  ( 31.50000000000000000, 40.03620104880000241, -137.0552959530000123 ) ) ;
#15814 = CARTESIAN_POINT ( 'NONE',  ( -35.33948162989999986, 16.82262754929999815, -143.5552959529999839 ) ) ;
#15815 = CARTESIAN_POINT ( 'NONE',  ( -24.90252082150000135, 32.60880315500000393, -143.5690609609999910 ) ) ;
#15816 = ORIENTED_EDGE ( 'NONE', *, *, #9701, .F. ) ;
#15817 = DIRECTION ( 'NONE',  ( 1.000000000000000000, 0.000000000000000000, 2.516505522483685870E-12 ) ) ;
#15818 = DIRECTION ( 'NONE',  ( 2.507771768019999718E-12, 1.592654864069999939E-17, -1.000000000000000000 ) ) ;
#15819 = EDGE_CURVE ( 'NONE', #23304, #70, #8571, .T. ) ;
#15820 = CARTESIAN_POINT ( 'NONE',  ( -14.02405267930000043, 37.94700976039999318, -139.5674429869999926 ) ) ;
#15821 = DIRECTION ( 'NONE',  ( -1.000000000000000000, 0.000000000000000000, 2.245315044999999693E-12 ) ) ;
#15822 = AXIS2_PLACEMENT_3D ( 'NONE', #21244, #23140, #6709 ) ;
#15823 = ORIENTED_EDGE ( 'NONE', *, *, #7065, .T. ) ;
#15824 = DIRECTION ( 'NONE',  ( -2.508215857230000030E-12, 0.000000000000000000, 1.000000000000000000 ) ) ;
#15825 = LINE ( 'NONE', #6777, #20355 ) ;
#15826 = PLANE ( 'NONE',  #8745 ) ;
#15827 = DIRECTION ( 'NONE',  ( -1.000000000000000000, 0.000000000000000000, 2.257144641399999941E-12 ) ) ;
#15828 = PLANE ( 'NONE',  #19826 ) ;
#15829 = CARTESIAN_POINT ( 'NONE',  ( 2.499999999879999990, -3.500000000000000000, -135.0552959530000123 ) ) ;
#15830 = ORIENTED_EDGE ( 'NONE', *, *, #7098, .T. ) ;
#15831 = CARTESIAN_POINT ( 'NONE',  ( -16.26018138119240675, 34.43780680547004636, -140.2208411054963619 ) ) ;
#15832 = CARTESIAN_POINT ( 'NONE',  ( -9.347107914279998653, -17.32706600430000066, -144.5552959529999839 ) ) ;
#15833 = CARTESIAN_POINT ( 'NONE',  ( -3.500000000000000000, 46.50000000000000000, -151.0552959529999839 ) ) ;
#15834 = CARTESIAN_POINT ( 'NONE',  ( 23.93638409349999918, -31.59322175579999836, -144.0552959529999839 ) ) ;
#15835 = LINE ( 'NONE', #6319, #5847 ) ;
#15836 = VERTEX_POINT ( 'NONE', #11558 ) ;
#15837 = DIRECTION ( 'NONE',  ( 4.510774274156380201E-12, -1.321907670943998010E-13, 1.000000000000000000 ) ) ;
#15838 = CIRCLE ( 'NONE', #19652, 7.499999999999999112 ) ;
#15839 = CARTESIAN_POINT ( 'NONE',  ( -25.64408091310000160, 33.16124342930000068, -144.5387451670000019 ) ) ;
#15840 = VERTEX_POINT ( 'NONE', #2782 ) ;
#15841 = CARTESIAN_POINT ( 'NONE',  ( -28.90798551742755862, 37.01360947635620136, -139.5686590453623808 ) ) ;
#15842 = DIRECTION ( 'NONE',  ( -0.1778629393740580045, -0.9840552701943220404, 3.562475540061165072E-13 ) ) ;
#15843 = ORIENTED_EDGE ( 'NONE', *, *, #9064, .F. ) ;
#15844 = EDGE_CURVE ( 'NONE', #1, #20629, #4789, .T. ) ;
#15845 = CARTESIAN_POINT ( 'NONE',  ( -13.49610831274083189, 36.09202739918482195, -139.6200137135016064 ) ) ;
#15846 = ADVANCED_FACE ( 'NONE', ( #2439 ), #2544, .F. ) ;
#15847 = DIRECTION ( 'NONE',  ( 1.000000000000000000, 0.000000000000000000, -2.256131789327549967E-12 ) ) ;
#15848 = DIRECTION ( 'NONE',  ( -1.000000000000000000, -2.602084704489999637E-17, 1.701177084830000066E-20 ) ) ;
#15849 = CARTESIAN_POINT ( 'NONE',  ( 7.190767566730844607, 36.26753466208879928, -141.6649243765320421 ) ) ;
#15850 = VERTEX_POINT ( 'NONE', #11448 ) ;
#15851 = CARTESIAN_POINT ( 'NONE',  ( -10.28506259363968844, 34.15285781884922045, -147.7829287822364961 ) ) ;
#15852 = EDGE_CURVE ( 'NONE', #14794, #4187, #9767, .T. ) ;
#15853 = PLANE ( 'NONE',  #19601 ) ;
#15854 = AXIS2_PLACEMENT_3D ( 'NONE', #3999, #11349, #2346 ) ;
#15855 = CARTESIAN_POINT ( 'NONE',  ( -8.743032712512970761, 39.11948877732287144, -147.0257656743172845 ) ) ;
#15856 = DIRECTION ( 'NONE',  ( -0.000000000000000000, 1.000000000000000000, 0.000000000000000000 ) ) ;
#15857 = ORIENTED_EDGE ( 'NONE', *, *, #19892, .F. ) ;
#15858 =( NAMED_UNIT ( * ) SI_UNIT ( $, .STERADIAN. ) SOLID_ANGLE_UNIT ( ) );
#15859 = ORIENTED_EDGE ( 'NONE', *, *, #9190, .F. ) ;
#15860 = CARTESIAN_POINT ( 'NONE',  ( -7.249489785462221114, 33.98920719456333472, -145.9090368077603443 ) ) ;
#15861 = CARTESIAN_POINT ( 'NONE',  ( -22.62924774399999706, 37.91877106609999970, -140.0196664479999811 ) ) ;
#15862 = CARTESIAN_POINT ( 'NONE',  ( -2.500000000000000000, 40.00000000000000000, -150.0552959529999839 ) ) ;
#15863 = VERTEX_POINT ( 'NONE', #22290 ) ;
#15864 = CARTESIAN_POINT ( 'NONE',  ( -12.50000000000000000, 19.50000000000000000, -136.0552959530000123 ) ) ;
#15865 = FACE_OUTER_BOUND ( 'NONE', #12646, .T. ) ;
#15866 = ORIENTED_EDGE ( 'NONE', *, *, #10973, .T. ) ;
#15867 = DIRECTION ( 'NONE',  ( -2.507771768023035002E-12, -1.592654560756634986E-17, 1.000000000000000000 ) ) ;
#15868 = AXIS2_PLACEMENT_3D ( 'NONE', #7131, #13068, #14391 ) ;
#15869 = DIRECTION ( 'NONE',  ( 0.7401352420267017784, 0.6724580459107286634, -3.250177904590145368E-12 ) ) ;
#15870 = CIRCLE ( 'NONE', #11674, 1.000000000000000888 ) ;
#15871 = FACE_OUTER_BOUND ( 'NONE', #5250, .T. ) ;
#15872 = CARTESIAN_POINT ( 'NONE',  ( 6.000000000140000012, 41.50000000000000000, -147.5552959529999839 ) ) ;
#15873 = EDGE_CURVE ( 'NONE', #10865, #20660, #13471, .T. ) ;
#15874 = CARTESIAN_POINT ( 'NONE',  ( 16.52685120005601149, -19.88477712180281998, -143.5552959530023145 ) ) ;
#15875 = LINE ( 'NONE', #23145, #8600 ) ;
#15876 = FACE_OUTER_BOUND ( 'NONE', #4035, .T. ) ;
#15877 = ADVANCED_FACE ( 'NONE', ( #15027 ), #17285, .T. ) ;
#15878 = LINE ( 'NONE', #6837, #3991 ) ;
#15879 = SHAPE_REPRESENTATION ( 'Phillips Screw', ( #5025 ), #9222 ) ;
#15880 = ORIENTED_EDGE ( 'NONE', *, *, #13206, .F. ) ;
#15881 = CARTESIAN_POINT ( 'NONE',  ( -32.50000000000000000, -36.00000000000000000, -150.5552959529999839 ) ) ;
#15882 = UNCERTAINTY_MEASURE_WITH_UNIT (LENGTH_MEASURE( 1.000000000000000082E-05 ), #6140, 'distance_accuracy_value', 'NONE');
#15884 = ORIENTED_EDGE ( 'NONE', *, *, #9181, .T. ) ;
#15883 = VECTOR ( 'NONE', #22269, 1000.000000000000114 ) ;
#15885 = FILL_AREA_STYLE ('',( #6722 ) ) ;
#15886 = AXIS2_PLACEMENT_3D ( 'NONE', #12309, #12068, #15770 ) ;
#15887 = ORIENTED_EDGE ( 'NONE', *, *, #2391, .T. ) ;
#15888 = DIRECTION ( 'NONE',  ( -8.956391184260000029E-12, 9.094947017729999296E-13, -1.000000000000000000 ) ) ;
#15889 = CARTESIAN_POINT ( 'NONE',  ( -8.594304764349999459, -10.75357442870000035, -144.5552959529999839 ) ) ;
#15890 = ORIENTED_EDGE ( 'NONE', *, *, #23355, .T. ) ;
#15891 = ORIENTED_EDGE ( 'NONE', *, *, #16514, .F. ) ;
#15892 = LINE ( 'NONE', #3758, #14421 ) ;
#15893 = CARTESIAN_POINT ( 'NONE',  ( -8.810109936750000870, 39.32487244789999892, -140.7337397739999858 ) ) ;
#15894 = DIRECTION ( 'NONE',  ( 0.000000000000000000, -1.000000000000000000, 0.000000000000000000 ) ) ;
#15895 = CARTESIAN_POINT ( 'NONE',  ( 24.75935218339999722, -28.32938697159999819, -146.5552959529999839 ) ) ;
#15896 = CARTESIAN_POINT ( 'NONE',  ( -7.220568065030000149, 34.52259161599999970, -140.6708207100000152 ) ) ;
#15897 = EDGE_CURVE ( 'NONE', #19149, #10191, #23047, .T. ) ;
#15898 = ORIENTED_EDGE ( 'NONE', *, *, #4992, .F. ) ;
#15899 = CARTESIAN_POINT ( 'NONE',  ( 9.077094367341661751, 35.61544623144256150, -141.9737733526287116 ) ) ;
#15900 = AXIS2_PLACEMENT_3D ( 'NONE', #21966, #10001, #22633 ) ;
#15901 = CIRCLE ( 'NONE', #21994, 35.00000000000000000 ) ;
#15902 = DIRECTION ( 'NONE',  ( 1.000000000000000000, 2.602084704489999637E-17, -1.701177084830000066E-20 ) ) ;
#15903 = AXIS2_PLACEMENT_3D ( 'NONE', #14664, #5066, #4948 ) ;
#15904 = DIRECTION ( 'NONE',  ( -1.000000000000000000, 0.000000000000000000, 2.257120985840000117E-12 ) ) ;
#15905 = EDGE_CURVE ( 'NONE', #10363, #22236, #6309, .T. ) ;
#15906 = ORIENTED_EDGE ( 'NONE', *, *, #8125, .T. ) ;
#15907 = AXIS2_PLACEMENT_3D ( 'NONE', #851, #20249, #18563 ) ;
#15908 = DIRECTION ( 'NONE',  ( 0.7071067811865484609, 0.7071067811865466846, 1.776356839400247234E-12 ) ) ;
#15909 = ORIENTED_EDGE ( 'NONE', *, *, #11522, .F. ) ;
#15910 = PLANE ( 'NONE',  #18558 ) ;
#15911 = LINE ( 'NONE', #4854, #12363 ) ;
#15912 = ORIENTED_EDGE ( 'NONE', *, *, #15989, .F. ) ;
#15913 = DIRECTION ( 'NONE',  ( 3.994014902950000436E-29, -1.000000000000000000, 4.148443855749999753E-27 ) ) ;
#15914 = CARTESIAN_POINT ( 'NONE',  ( -11.97832217620000073, 39.59660284089999749, -147.8163995769999985 ) ) ;
#15915 = VERTEX_POINT ( 'NONE', #4086 ) ;
#15916 = CARTESIAN_POINT ( 'NONE',  ( -15.66511667654221718, 38.49419402878272933, -147.3083789397792316 ) ) ;
#15917 = ADVANCED_FACE ( 'NONE', ( #4557 ), #639, .T. ) ;
#15918 = CARTESIAN_POINT ( 'NONE',  ( -4.510096969185095617, 46.24633263602936495, -136.0552959529898374 ) ) ;
#15919 = ORIENTED_EDGE ( 'NONE', *, *, #3537, .T. ) ;
#15920 =( NAMED_UNIT ( * ) SI_UNIT ( $, .STERADIAN. ) SOLID_ANGLE_UNIT ( ) );
#15921 = AXIS2_PLACEMENT_3D ( 'NONE', #15460, #13913, #17362 ) ;
#15922 = ORIENTED_EDGE ( 'NONE', *, *, #2753, .T. ) ;
#15923 = DIRECTION ( 'NONE',  ( 2.507771768019999718E-12, 1.592654864209999947E-17, -1.000000000000000000 ) ) ;
#15924 = VECTOR ( 'NONE', #9037, 1000.000000000000227 ) ;
#15925 = FACE_BOUND ( 'NONE', #19612, .T. ) ;
#15926 = VERTEX_POINT ( 'NONE', #18949 ) ;
#15927 = LINE ( 'NONE', #14381, #6081 ) ;
#15928 = VECTOR ( 'NONE', #5824, 1000.000000000000000 ) ;
#15929 = EDGE_CURVE ( 'NONE', #3173, #8776, #5862, .T. ) ;
#15930 = AXIS2_PLACEMENT_3D ( 'NONE', #21750, #14944, #7336 ) ;
#15931 = CARTESIAN_POINT ( 'NONE',  ( 1.133692148550000001, -51.50000000000000000, -134.3952035990000127 ) ) ;
#15932 = ORIENTED_EDGE ( 'NONE', *, *, #5745, .T. ) ;
#15933 = EDGE_CURVE ( 'NONE', #2396, #22806, #13121, .T. ) ;
#15934 = LINE ( 'NONE', #23198, #1091 ) ;
#15935 = ADVANCED_FACE ( 'NONE', ( #18603 ), #2321, .F. ) ;
#15936 = ADVANCED_FACE ( 'NONE', ( #14072 ), #10475, .F. ) ;
#15937 = ORIENTED_EDGE ( 'NONE', *, *, #5828, .T. ) ;
#15938 = FACE_OUTER_BOUND ( 'NONE', #4615, .T. ) ;
#15939 = AXIS2_PLACEMENT_3D ( 'NONE', #2080, #5517, #12766 ) ;
#15940 = PLANE ( 'NONE',  #15011 ) ;
#15941 = VECTOR ( 'NONE', #3951, 1000.000000000000000 ) ;
#15942 = CARTESIAN_POINT ( 'NONE',  ( -14.64556842670265802, 38.56874084764600497, -147.7756864782241166 ) ) ;
#15943 = LINE ( 'NONE', #12355, #3031 ) ;
#15944 = ORIENTED_EDGE ( 'NONE', *, *, #1474, .T. ) ;
#15945 = DIRECTION ( 'NONE',  ( 0.000000000000000000, 1.000000000000000000, 0.000000000000000000 ) ) ;
#15946 = DIRECTION ( 'NONE',  ( -0.1000233216789610108, -0.9949850929136109245, 3.591470555298595137E-13 ) ) ;
#15947 = VECTOR ( 'NONE', #5565, 1000.000000000000000 ) ;
#15948 = LINE ( 'NONE', #12015, #21290 ) ;
#15949 = CARTESIAN_POINT ( 'NONE',  ( 7.133692148549999779, 51.50000000000000000, -137.0552959530000123 ) ) ;
#15950 = CARTESIAN_POINT ( 'NONE',  ( -24.84704225926845922, 37.03879906168354097, -147.5513581853375058 ) ) ;
#15951 = CIRCLE ( 'NONE', #14048, 1.499999999999999556 ) ;
#15952 = PLANE ( 'NONE',  #8301 ) ;
#15953 = VECTOR ( 'NONE', #16543, 1000.000000000000000 ) ;
#15954 = ORIENTED_EDGE ( 'NONE', *, *, #14297, .F. ) ;
#15955 = DIRECTION ( 'NONE',  ( 5.094701932209999624E-24, 1.000000000000000000, 0.000000000000000000 ) ) ;
#15956 = FACE_OUTER_BOUND ( 'NONE', #6895, .T. ) ;
#15957 = FACE_OUTER_BOUND ( 'NONE', #7520, .T. ) ;
#15958 = CARTESIAN_POINT ( 'NONE',  ( -6.705189174532299567, 39.56570632385503927, -147.4373625593833879 ) ) ;
#15959 = DIRECTION ( 'NONE',  ( 2.257157423930000049E-12, 0.000000000000000000, 1.000000000000000000 ) ) ;
#15960 = CARTESIAN_POINT ( 'NONE',  ( 4.468795199060000556, -26.40504320680000205, -142.5552959529999839 ) ) ;
#15961 = ORIENTED_EDGE ( 'NONE', *, *, #10212, .F. ) ;
#15962 = DIRECTION ( 'NONE',  ( 2.257144641397284947E-12, 2.714760815920564689E-24, 1.000000000000000000 ) ) ;
#15963 = EDGE_CURVE ( 'NONE', #3707, #9912, #17751, .T. ) ;
#15964 = CARTESIAN_POINT ( 'NONE',  ( 19.00000000000000000, 39.50000000000000000, -137.0552959530000123 ) ) ;
#15965 = EDGE_LOOP ( 'NONE', ( #23011, #18402, #22630, #6198 ) ) ;
#15966 = AXIS2_PLACEMENT_3D ( 'NONE', #14045, #2869, #10103 ) ;
#15967 = AXIS2_PLACEMENT_3D ( 'NONE', #6238, #18970, #15756 ) ;
#15968 = CIRCLE ( 'NONE', #7599, 2.600000000000000089 ) ;
#15969 = DIRECTION ( 'NONE',  ( -0.000000000000000000, 1.000000000000000000, 0.000000000000000000 ) ) ;
#15970 = ORIENTED_EDGE ( 'NONE', *, *, #199, .F. ) ;
#15971 = CARTESIAN_POINT ( 'NONE',  ( -10.01911575600000148, -21.69748113039999637, -148.0552959529999839 ) ) ;
#15972 = LINE ( 'NONE', #6686, #12380 ) ;
#15973 = CARTESIAN_POINT ( 'NONE',  ( 31.00000000000000000, -39.80430157320000006, -151.0552959529999839 ) ) ;
#15974 = CARTESIAN_POINT ( 'NONE',  ( 7.443892100749126328, 38.06519908407426556, -141.7935801463240182 ) ) ;
#15975 = EDGE_LOOP ( 'NONE', ( #19617, #20812, #6289, #18447 ) ) ;
#15976 = CARTESIAN_POINT ( 'NONE',  ( -10.13678785082237077, 32.34748245543284639, -143.2747856603235732 ) ) ;
#15977 = CARTESIAN_POINT ( 'NONE',  ( -17.91974642295373599, 36.92811127467410159, -148.3783205066400797 ) ) ;
#15978 = CARTESIAN_POINT ( 'NONE',  ( 23.99773978629999860, -29.25880395889999974, -147.5552959529999839 ) ) ;
#15979 = CARTESIAN_POINT ( 'NONE',  ( 4.523700915383287224, -35.78365992287999120, -136.0552959530101589 ) ) ;
#15980 = ORIENTED_EDGE ( 'NONE', *, *, #12099, .T. ) ;
#15981 = VECTOR ( 'NONE', #15574, 1000.000000000000000 ) ;
#15982 = AXIS2_PLACEMENT_3D ( 'NONE', #12528, #3504, #8952 ) ;
#15983 = CARTESIAN_POINT ( 'NONE',  ( 17.88103053862789693, 20.98519100496283940, -136.0552959530403996 ) ) ;
#15984 = ORIENTED_EDGE ( 'NONE', *, *, #18567, .T. ) ;
#15985 = CARTESIAN_POINT ( 'NONE',  ( -6.578755062799197084, 35.62001169219931995, -147.2160746728349920 ) ) ;
#15986 = CARTESIAN_POINT ( 'NONE',  ( 31.50000000030000180, -40.03620104859999884, -150.0552959529999839 ) ) ;
#15987 = FACE_OUTER_BOUND ( 'NONE', #18440, .T. ) ;
#15988 = VERTEX_POINT ( 'NONE', #2896 ) ;
#15989 = EDGE_CURVE ( 'NONE', #21976, #10060, #17521, .T. ) ;
#15990 = CYLINDRICAL_SURFACE ( 'NONE', #3811, 1.500000000000001332 ) ;
#15991 = LINE ( 'NONE', #23252, #12149 ) ;
#15992 = VERTEX_POINT ( 'NONE', #23232 ) ;
#15993 = CARTESIAN_POINT ( 'NONE',  ( -17.01025018560000035, 38.48180121059999692, -140.7067500819999850 ) ) ;
#15994 = PLANE ( 'NONE',  #20110 ) ;
#15995 = CARTESIAN_POINT ( 'NONE',  ( 18.95053822279999878, -51.50000000000000000, -149.8052959529999839 ) ) ;
#15996 = CIRCLE ( 'NONE', #5733, 1.499999999999996225 ) ;
#15997 = VECTOR ( 'NONE', #6048, 1000.000000000000000 ) ;
#15998 = CARTESIAN_POINT ( 'NONE',  ( 26.50000000000000000, -20.50000000000000000, -137.0552959530000123 ) ) ;
#15999 = COLOUR_RGB ( '', 0.40784314, 0.44705882, 0.49803922) ;
#16000 = CARTESIAN_POINT ( 'NONE',  ( -3.499999999959999997, 44.50000000000000000, -136.0552959530000123 ) ) ;
#16001 = CARTESIAN_POINT ( 'NONE',  ( -9.934356875269999776, -23.16624500709999879, -146.5552959529999839 ) ) ;
#16002 = ITEM_DEFINED_TRANSFORMATION ( 'NONE', 'NONE', #10375,  #5025 ) ;
#16003 = DIRECTION ( 'NONE',  ( -2.602084704489999637E-17, 1.000000000000000000, 0.000000000000000000 ) ) ;
#16004 = DIRECTION ( 'NONE',  ( 0.000000000000000000, 0.000000000000000000, 1.000000000000000000 ) ) ;
#16005 = EDGE_LOOP ( 'NONE', ( #17916, #8687, #9108, #14740 ) ) ;
#16006 = CARTESIAN_POINT ( 'NONE',  ( -32.50000000000000000, 47.50000000000000000, -137.0552959530000123 ) ) ;
#16007 = EDGE_LOOP ( 'NONE', ( #13821, #11866, #20226, #3603 ) ) ;
#16008 = SURFACE_STYLE_USAGE ( .BOTH. , #8734 ) ;
#16009 = ORIENTED_EDGE ( 'NONE', *, *, #11345, .F. ) ;
#16010 = CARTESIAN_POINT ( 'NONE',  ( -16.26554697147297190, 36.25315601839098889, -147.8310094943498711 ) ) ;
#16011 = CARTESIAN_POINT ( 'NONE',  ( -28.14969746252968008, 32.41805236243940413, -143.4814202872574072 ) ) ;
#16012 = CARTESIAN_POINT ( 'NONE',  ( 8.100000000049998761, 39.46779253580000102, -148.7552959530000010 ) ) ;
#16013 = AXIS2_PLACEMENT_3D ( 'NONE', #2871, #20837, #8093 ) ;
#16014 = VECTOR ( 'NONE', #7774, 1000.000000000000000 ) ;
#16015 = CARTESIAN_POINT ( 'NONE',  ( 1.000000000160000013, 41.50000000000000000, -140.5552959529999839 ) ) ;
#16016 = VECTOR ( 'NONE', #1226, 1000.000000000000000 ) ;
#16017 = ORIENTED_EDGE ( 'NONE', *, *, #15140, .F. ) ;
#16018 = EDGE_CURVE ( 'NONE', #7005, #18905, #8575, .T. ) ;
#16019 = DIRECTION ( 'NONE',  ( 0.7633862853691523176, -0.6459422414661291079, 0.000000000000000000 ) ) ;
#16020 = CARTESIAN_POINT ( 'NONE',  ( -19.07874927058154668, 33.55317438757552395, -144.5781697712094171 ) ) ;
#16021 = CARTESIAN_POINT ( 'NONE',  ( 7.133692148549999779, -51.50000000000000000, -137.0552959530000123 ) ) ;
#16022 = EDGE_CURVE ( 'NONE', #12006, #20679, #10100, .T. ) ;
#16023 = DIRECTION ( 'NONE',  ( -2.257171095940000041E-12, -1.003664318210000046E-28, -1.000000000000000000 ) ) ;
#16024 = ORIENTED_EDGE ( 'NONE', *, *, #20195, .T. ) ;
#16025 = CARTESIAN_POINT ( 'NONE',  ( 22.40528270640000130, -21.39206583629999869, -146.5552959529999839 ) ) ;
#16026 =( REPRESENTATION_RELATIONSHIP ('NONE','NONE', #7672, #15114 ) REPRESENTATION_RELATIONSHIP_WITH_TRANSFORMATION ( #5523 )SHAPE_REPRESENTATION_RELATIONSHIP( ) );
#16027 = ORIENTED_EDGE ( 'NONE', *, *, #19235, .T. ) ;
#16028 = CARTESIAN_POINT ( 'NONE',  ( 9.872691270914929262, 36.39514331228942012, -141.6295540220486089 ) ) ;
#16029 =( BOUNDED_CURVE ( )  B_SPLINE_CURVE ( 5, ( #16410, #5348, #17840, #10792, #18075, #8777, #14513, #10679, #3798, #7125, #14387, #5103 ),
 .UNSPECIFIED., .F., .F. ) 
 B_SPLINE_CURVE_WITH_KNOTS ( ( 6, 3, 3, 6 ),
 ( 0.000000000000000000, 4.358589029760000066, 8.533830367689999363, 12.54112731390000057 ),
 .UNSPECIFIED. ) 
 CURVE ( )  GEOMETRIC_REPRESENTATION_ITEM ( )  RATIONAL_B_SPLINE_CURVE ( ( 0.2500000000000000000, 0.2500000000000000000, 0.2500000000000000000, 0.2500000000000000000, 0.2500000000000000000, 0.2500000000000000000, 0.2500000000000000000, 0.2500000000000000000, 0.2500000000000000000, 0.2500000000000000000, 0.2500000000000000000, 0.2500000000000000000 ) ) 
 REPRESENTATION_ITEM ( '' )  );
#16030 = CARTESIAN_POINT ( 'NONE',  ( 6.500000000040000003, 20.50000000000000000, -136.0552959530000123 ) ) ;
#16031 = CARTESIAN_POINT ( 'NONE',  ( -20.60824191589999899, -32.00000000000000000, -145.5657682190000060 ) ) ;
#16032 = VECTOR ( 'NONE', #11739, 1000.000000000000000 ) ;
#16033 = ORIENTED_EDGE ( 'NONE', *, *, #8774, .F. ) ;
#16034 = AXIS2_PLACEMENT_3D ( 'NONE', #14691, #20184, #11334 ) ;
#16035 = DIRECTION ( 'NONE',  ( 1.000000000000000000, 0.000000000000000000, -1.527536832333224173E-13 ) ) ;
#16036 = ORIENTED_EDGE ( 'NONE', *, *, #20750, .F. ) ;
#16037 = CARTESIAN_POINT ( 'NONE',  ( -33.00000000000000000, 37.00000000000000000, -149.5552959529999839 ) ) ;
#16038 = CARTESIAN_POINT ( 'NONE',  ( -38.50000000000000000, 26.50000000000000000, -149.5552959529999839 ) ) ;
#16039 = VERTEX_POINT ( 'NONE', #12036 ) ;
#16040 = DIRECTION ( 'NONE',  ( -0.1000233216789610108, -0.9949850929136109245, 3.576398436658600095E-13 ) ) ;
#16041 = VERTEX_POINT ( 'NONE', #6804 ) ;
#16042 = CARTESIAN_POINT ( 'NONE',  ( -16.16658683009993069, 37.07694188521394096, -148.2333767341113742 ) ) ;
#16043 = PLANE ( 'NONE',  #16723 ) ;
#16044 = ORIENTED_EDGE ( 'NONE', *, *, #13030, .F. ) ;
#16045 = SURFACE_STYLE_FILL_AREA ( #10547 ) ;
#16046 = ORIENTED_EDGE ( 'NONE', *, *, #4201, .T. ) ;
#16047 = PRODUCT_DEFINITION_SHAPE ( 'NONE', 'NONE',  #16194 ) ;
#16048 = CARTESIAN_POINT ( 'NONE',  ( -26.81163552868969191, 38.56513266870371837, -140.3212796651035319 ) ) ;
#16049 = CARTESIAN_POINT ( 'NONE',  ( 16.26251912989999937, -22.62374141290000296, -144.5552959529999839 ) ) ;
#16050 = ORIENTED_EDGE ( 'NONE', *, *, #4008, .T. ) ;
#16051 = AXIS2_PLACEMENT_3D ( 'NONE', #11622, #13789, #22832 ) ;
#16052 = ADVANCED_FACE ( 'NONE', ( #19429 ), #3135, .F. ) ;
#16053 = DIRECTION ( 'NONE',  ( 0.000000000000000000, 0.000000000000000000, 1.000000000000000000 ) ) ;
#16054 = VECTOR ( 'NONE', #5796, 1000.000000000000000 ) ;
#16055 = CARTESIAN_POINT ( 'NONE',  ( 4.750000000000000000, 0.000000000000000000, -150.0552959529999839 ) ) ;
#16056 = ORIENTED_EDGE ( 'NONE', *, *, #6029, .F. ) ;
#16057 = LINE ( 'NONE', #7248, #8682 ) ;
#16058 = EDGE_CURVE ( 'NONE', #22265, #8748, #19217, .T. ) ;
#16059 = ORIENTED_EDGE ( 'NONE', *, *, #12402, .T. ) ;
#16060 = LINE ( 'NONE', #5352, #272 ) ;
#16061 = DIRECTION ( 'NONE',  ( -0.1000233216789610108, -0.9949850929136109245, 3.600083194518594546E-13 ) ) ;
#16062 = CARTESIAN_POINT ( 'NONE',  ( -13.50483231551108609, 37.84550326251047636, -140.3648548379449892 ) ) ;
#16063 = DIRECTION ( 'NONE',  ( 0.000000000000000000, 0.000000000000000000, 1.000000000000000000 ) ) ;
#16064 = ORIENTED_EDGE ( 'NONE', *, *, #17540, .F. ) ;
#16065 = CARTESIAN_POINT ( 'NONE',  ( 3.175226512005099533, 13.75903940329188480, -136.0552959530071746 ) ) ;
#16066 = PRESENTATION_LAYER_ASSIGNMENT (  '', '', ( #5419 ) ) ;
#16067 = CARTESIAN_POINT ( 'NONE',  ( -31.00000000000000000, -43.00000000000000000, -151.0552959529999839 ) ) ;
#16068 = AXIS2_PLACEMENT_3D ( 'NONE', #23159, #6732, #6853 ) ;
#16069 = EDGE_CURVE ( 'NONE', #2852, #919, #19659, .T. ) ;
#16070 = DIRECTION ( 'NONE',  ( 1.211690350419999855E-27, 2.765629237170000203E-27, -1.000000000000000000 ) ) ;
#16071 = CARTESIAN_POINT ( 'NONE',  ( -32.50000000000000000, -51.00000000000000000, -136.0552959530000123 ) ) ;
#16072 = DIRECTION ( 'NONE',  ( 0.06298685227120542907, 0.9980143568310855251, -1.492139745100128694E-13 ) ) ;
#16073 = DIRECTION ( 'NONE',  ( 0.000000000000000000, 1.000000000000000000, 0.000000000000000000 ) ) ;
#16074 = ADVANCED_FACE ( 'NONE', ( #3353 ), #5133, .T. ) ;
#16075 = ORIENTED_EDGE ( 'NONE', *, *, #13677, .T. ) ;
#16076 = EDGE_CURVE ( 'NONE', #3657, #10194, #1468, .T. ) ;
#16077 = CARTESIAN_POINT ( 'NONE',  ( 16.74346552629999962, -18.31657829129999726, -148.5552959529999839 ) ) ;
#16078 = CARTESIAN_POINT ( 'NONE',  ( -13.13790626639999992, 32.38985286280000508, -143.7114742199999853 ) ) ;
#16079 = EDGE_CURVE ( 'NONE', #2684, #10468, #15972, .T. ) ;
#16080 = CARTESIAN_POINT ( 'NONE',  ( -5.268406987068996017, 41.62455876149470413, -143.5667302874617235 ) ) ;
#16081 = FACE_OUTER_BOUND ( 'NONE', #22561, .T. ) ;
#16082 = DIRECTION ( 'NONE',  ( 0.000000000000000000, 0.000000000000000000, 1.000000000000000000 ) ) ;
#16083 = ORIENTED_EDGE ( 'NONE', *, *, #14940, .T. ) ;
#16084 = CARTESIAN_POINT ( 'NONE',  ( -26.39607007120000048, 36.95534867429999792, -140.3840478969999879 ) ) ;
#16085 = DIRECTION ( 'NONE',  ( -2.602084747549999882E-17, 1.000000000000000000, 5.873289694040000105E-29 ) ) ;
#16086 = ORIENTED_EDGE ( 'NONE', *, *, #16824, .T. ) ;
#16087 = EDGE_CURVE ( 'NONE', #8740, #15695, #13946, .T. ) ;
#16088 = FACE_OUTER_BOUND ( 'NONE', #12245, .T. ) ;
#16089 = ORIENTED_EDGE ( 'NONE', *, *, #2786, .F. ) ;
#16090 = EDGE_CURVE ( 'NONE', #18121, #10865, #15431, .T. ) ;
#16091 = DIRECTION ( 'NONE',  ( 0.000000000000000000, 0.000000000000000000, 1.000000000000000000 ) ) ;
#16092 = CARTESIAN_POINT ( 'NONE',  ( -29.43227084506111879, 38.18732975763461468, -139.4730824933273539 ) ) ;
#16093 = CARTESIAN_POINT ( 'NONE',  ( 6.000000000160000013, 29.48610037779999971, -140.0552959529999839 ) ) ;
#16094 = CARTESIAN_POINT ( 'NONE',  ( 7.319978021535112234, 37.92635072559305343, -141.7332369987670404 ) ) ;
#16095 = ORIENTED_EDGE ( 'NONE', *, *, #4732, .F. ) ;
#16096 = CARTESIAN_POINT ( 'NONE',  ( -10.88504013576124585, 37.01634837950538071, -139.4704149077313673 ) ) ;
#16097 = CARTESIAN_POINT ( 'NONE',  ( -30.49999999990000177, 37.00000000000000000, -144.0552959529999839 ) ) ;
#16098 = EDGE_CURVE ( 'NONE', #19591, #4852, #17335, .T. ) ;
#16099 = CARTESIAN_POINT ( 'NONE',  ( -8.931798216462233597, 36.92954985151496317, -147.9669232058025159 ) ) ;
#16100 = CARTESIAN_POINT ( 'NONE',  ( 9.763108217368069219, -33.86272049728325584, -136.0552959530220392 ) ) ;
#16101 = ORIENTED_EDGE ( 'NONE', *, *, #1029, .F. ) ;
#16102 = ADVANCED_FACE ( 'NONE', ( #8227 ), #15498, .T. ) ;
#16103 = EDGE_CURVE ( 'NONE', #23517, #6964, #13270, .T. ) ;
#16104 = CARTESIAN_POINT ( 'NONE',  ( 18.66051412337919757, 24.90191174485666181, -136.0552959530421617 ) ) ;
#16105 =( LENGTH_UNIT ( ) NAMED_UNIT ( * ) SI_UNIT ( .MILLI., .METRE. ) );
#16106 = EDGE_CURVE ( 'NONE', #4774, #15020, #20988, .T. ) ;
#16107 = VECTOR ( 'NONE', #15043, 1000.000000000000000 ) ;
#16108 = ORIENTED_EDGE ( 'NONE', *, *, #22879, .F. ) ;
#16109 = FACE_OUTER_BOUND ( 'NONE', #13090, .T. ) ;
#16110 = PLANE ( 'NONE',  #10330 ) ;
#16111 = CARTESIAN_POINT ( 'NONE',  ( -5.660609041603422931, 24.90181682660472973, -136.0552959529872510 ) ) ;
#16112 = ORIENTED_EDGE ( 'NONE', *, *, #9840, .F. ) ;
#16113 = FACE_OUTER_BOUND ( 'NONE', #19111, .T. ) ;
#16114 = DIRECTION ( 'NONE',  ( -1.000000000000000000, 0.000000000000000000, 0.000000000000000000 ) ) ;
#16115 = ORIENTED_EDGE ( 'NONE', *, *, #1122, .F. ) ;
#16116 = DIRECTION ( 'NONE',  ( 2.255973186040000320E-12, 0.000000000000000000, 1.000000000000000000 ) ) ;
#16117 = CARTESIAN_POINT ( 'NONE',  ( -18.48412402378637864, 36.99547888838029053, -147.4161207264589564 ) ) ;
#16118 = DIRECTION ( 'NONE',  ( 1.000000000000000000, 0.000000000000000000, -2.715621035259064790E-14 ) ) ;
#16119 = CARTESIAN_POINT ( 'NONE',  ( 8.750000000030000891, -44.75000000000000000, -136.0552959530000123 ) ) ;
#16120 = LINE ( 'NONE', #19685, #21122 ) ;
#16121 = VECTOR ( 'NONE', #15608, 1000.000000000000114 ) ;
#16122 = CARTESIAN_POINT ( 'NONE',  ( -25.46206384013188284, 37.06683745572571098, -140.4480127386118511 ) ) ;
#16123 = APPLICATION_PROTOCOL_DEFINITION ( 'draft international standard', 'automotive_design', 1998, #21353 ) ;
#16124 = DIRECTION ( 'NONE',  ( 1.000000000000000000, 0.000000000000000000, 0.000000000000000000 ) ) ;
#16125 = DIRECTION ( 'NONE',  ( 1.000000000000000000, 0.000000000000000000, -2.257453483404485235E-12 ) ) ;
#16126 = EDGE_CURVE ( 'NONE', #4966, #23428, #10126, .T. ) ;
#16127 = DIRECTION ( 'NONE',  ( 2.257749542879999954E-12, 0.000000000000000000, 1.000000000000000000 ) ) ;
#16128 = EDGE_LOOP ( 'NONE', ( #2193, #4689, #6408, #11623, #8310, #15980, #4813, #16566, #14388, #15422 ) ) ;
#16129 = EDGE_CURVE ( 'NONE', #2164, #9556, #14654, .T. ) ;
#16130 = UNCERTAINTY_MEASURE_WITH_UNIT (LENGTH_MEASURE( 1.000000000000000082E-05 ), #6696, 'distance_accuracy_value', 'NONE');
#16131 = VERTEX_POINT ( 'NONE', #9280 ) ;
#16132 = SURFACE_STYLE_FILL_AREA ( #15885 ) ;
#16133 = ORIENTED_EDGE ( 'NONE', *, *, #14763, .T. ) ;
#16134 = DIRECTION ( 'NONE',  ( -1.000000000000000000, 0.000000000000000000, 2.257144641399999941E-12 ) ) ;
#16135 = CARTESIAN_POINT ( 'NONE',  ( -12.66605126736717679, 36.07579439668360521, -148.6554523513628681 ) ) ;
#16136 = LINE ( 'NONE', #7884, #14896 ) ;
#16137 = CARTESIAN_POINT ( 'NONE',  ( 13.00952979664376130, 24.25756286941559026, -136.0552959530293720 ) ) ;
#16138 = EDGE_LOOP ( 'NONE', ( #15035, #21222, #2020, #22609 ) ) ;
#16139 = VECTOR ( 'NONE', #1697, 1000.000000000000000 ) ;
#16140 = CARTESIAN_POINT ( 'NONE',  ( -3.500000000000000000, 42.50000000000000000, -150.5552959529999839 ) ) ;
#16141 = CARTESIAN_POINT ( 'NONE',  ( -20.23971019809999916, 35.09018026569999904, -140.0771129649999978 ) ) ;
#16142 = CARTESIAN_POINT ( 'NONE',  ( -11.42599417689999974, 41.52668172479999953, -143.7505393120000292 ) ) ;
#16143 = DIRECTION ( 'NONE',  ( -1.000000000000000000, 5.094701932209999624E-24, 2.257144641399999941E-12 ) ) ;
#16144 = ORIENTED_EDGE ( 'NONE', *, *, #6128, .T. ) ;
#16145 = CARTESIAN_POINT ( 'NONE',  ( 31.96891336220000213, 40.94938100119999547, -149.5552959529999839 ) ) ;
#16146 = ORIENTED_EDGE ( 'NONE', *, *, #18960, .T. ) ;
#16147 = CARTESIAN_POINT ( 'NONE',  ( 10.00000222906343339, 37.09571658197103261, -141.5552923336952915 ) ) ;
#16148 = DIRECTION ( 'NONE',  ( -1.082120504314331458E-12, 0.8775825618903714265, -0.4794255386042053368 ) ) ;
#16149 = DIRECTION ( 'NONE',  ( 1.000000000000000000, 0.000000000000000000, -2.854859206178974232E-14 ) ) ;
#16150 = ORIENTED_EDGE ( 'NONE', *, *, #19842, .F. ) ;
#16151 = EDGE_CURVE ( 'NONE', #23331, #9544, #7503, .T. ) ;
#16152 = EDGE_CURVE ( 'NONE', #23322, #22094, #8926, .T. ) ;
#16153 = CARTESIAN_POINT ( 'NONE',  ( 1.172620240290000115, -63.19354141059999108, -146.0552959529999839 ) ) ;
#16154 = ORIENTED_EDGE ( 'NONE', *, *, #16494, .F. ) ;
#16155 = AXIS2_PLACEMENT_3D ( 'NONE', #13124, #7653, #12662 ) ;
#16156 = CARTESIAN_POINT ( 'NONE',  ( 8.900000000049999471, 37.00000000000000000, -148.7552959530000010 ) ) ;
#16157 = EDGE_CURVE ( 'NONE', #1069, #14517, #7280, .T. ) ;
#16158 = LINE ( 'NONE', #21517, #5191 ) ;
#16159 = ORIENTED_EDGE ( 'NONE', *, *, #10787, .T. ) ;
#16160 = DIRECTION ( 'NONE',  ( 1.000000000000000000, 0.000000000000000000, -2.255973186040000320E-12 ) ) ;
#16161 = ORIENTED_EDGE ( 'NONE', *, *, #4567, .F. ) ;
#16162 = CARTESIAN_POINT ( 'NONE',  ( -16.06600907547494828, 37.95602789737367289, -148.2176118107361162 ) ) ;
#16163 = CARTESIAN_POINT ( 'NONE',  ( -5.101475126912967006, 45.72676979428531041, -136.0552959529885015 ) ) ;
#16164 = ORIENTED_EDGE ( 'NONE', *, *, #22861, .F. ) ;
#16165 = DIRECTION ( 'NONE',  ( 1.000000000000000000, 0.000000000000000000, 0.000000000000000000 ) ) ;
#16166 = EDGE_LOOP ( 'NONE', ( #3071, #4057, #10054, #16086 ) ) ;
#16167 = CARTESIAN_POINT ( 'NONE',  ( -26.68542098469999857, 39.18140699330000132, -140.9632721460000084 ) ) ;
#16168 = PLANE ( 'NONE',  #4283 ) ;
#16169 = ORIENTED_EDGE ( 'NONE', *, *, #20273, .T. ) ;
#16170 = DIRECTION ( 'NONE',  ( 2.257144641399999941E-12, -8.049635416090000264E-35, 1.000000000000000000 ) ) ;
#16171 =( BOUNDED_CURVE ( )  B_SPLINE_CURVE ( 5, ( #21365, #3262, #15993, #21717, #23371, #16353, #23136, #56, #5406, #5156, #19807, #7306 ),
 .UNSPECIFIED., .F., .F. ) 
 B_SPLINE_CURVE_WITH_KNOTS ( ( 6, 3, 3, 6 ),
 ( 0.000000000000000000, 4.124045064660000648, 8.344666563069999654, 12.67057240369999782 ),
 .UNSPECIFIED. ) 
 CURVE ( )  GEOMETRIC_REPRESENTATION_ITEM ( )  RATIONAL_B_SPLINE_CURVE ( ( 0.2500000000000000000, 0.2500000000000000000, 0.2500000000000000000, 0.2500000000000000000, 0.2500000000000000000, 0.2500000000000000000, 0.2500000000000000000, 0.2500000000000000000, 0.2500000000000000000, 0.2500000000000000000, 0.2500000000000000000, 0.2500000000000000000 ) ) 
 REPRESENTATION_ITEM ( '' )  );
#16172 = DIRECTION ( 'NONE',  ( 1.000000000000000000, 0.000000000000000000, -1.498801083243961330E-13 ) ) ;
#16173 = DIRECTION ( 'NONE',  ( -1.000000000000000000, 1.734728570689999873E-18, 2.257171095940000041E-12 ) ) ;
#16174 = VERTEX_POINT ( 'NONE', #21813 ) ;
#16175 = DIRECTION ( 'NONE',  ( 0.000000000000000000, 0.000000000000000000, 1.000000000000000000 ) ) ;
#16176 = AXIS2_PLACEMENT_3D ( 'NONE', #736, #13447, #17262 ) ;
#16177 = VECTOR ( 'NONE', #13494, 1000.000000000000000 ) ;
#16178 = ORIENTED_EDGE ( 'NONE', *, *, #12136, .T. ) ;
#16179 = FACE_OUTER_BOUND ( 'NONE', #14337, .T. ) ;
#16180 = DIRECTION ( 'NONE',  ( 0.000000000000000000, -1.000000000000000000, 0.000000000000000000 ) ) ;
#16181 = CARTESIAN_POINT ( 'NONE',  ( -16.65675009045287069, 37.97791044233296276, -139.5816482416001350 ) ) ;
#16182 = CARTESIAN_POINT ( 'NONE',  ( 1.133692148650000009, -51.00000000000000000, -137.0552959530000123 ) ) ;
#16183 = VERTEX_POINT ( 'NONE', #14769 ) ;
#16184 = EDGE_CURVE ( 'NONE', #5292, #22593, #16551, .T. ) ;
#16185 = LINE ( 'NONE', #2148, #8949 ) ;
#16186 = DIRECTION ( 'NONE',  ( 4.430318231639999944E-12, -6.100259101500000139E-13, 1.000000000000000000 ) ) ;
#16187 = CARTESIAN_POINT ( 'NONE',  ( -22.10824191589999899, -1.500000000000000000, -146.3157682190000060 ) ) ;
#16188 = DIRECTION ( 'NONE',  ( 2.255973186040000320E-12, 0.000000000000000000, 1.000000000000000000 ) ) ;
#16189 = FACE_OUTER_BOUND ( 'NONE', #7951, .T. ) ;
#16190 = VECTOR ( 'NONE', #1684, 1000.000000000000000 ) ;
#16191 = VECTOR ( 'NONE', #12770, 1000.000000000000114 ) ;
#16192 = EDGE_LOOP ( 'NONE', ( #18499, #22242, #20772, #5444, #7240, #6673, #17255, #6254, #9644, #14402, #1843, #637 ) ) ;
#16193 = CARTESIAN_POINT ( 'NONE',  ( 3.780861691979999772, -4.816373842840000030, -139.5552959529999839 ) ) ;
#16194 = PRODUCT_DEFINITION ( 'UNKNOWN', '', #516, #5420 ) ;
#16195 = CARTESIAN_POINT ( 'NONE',  ( 9.183200060760000838, -6.500000000000000000, -150.0552959529999839 ) ) ;
#16196 = CARTESIAN_POINT ( 'NONE',  ( -13.02237250279999969, 32.42872598539999274, -144.6889042450000034 ) ) ;
#16197 = EDGE_CURVE ( 'NONE', #802, #5378, #4044, .T. ) ;
#16198 = CARTESIAN_POINT ( 'NONE',  ( -4.875412749849999727, 39.32116320210000282, -140.9191069839999955 ) ) ;
#16199 = FACE_OUTER_BOUND ( 'NONE', #20254, .T. ) ;
#16200 = ORIENTED_EDGE ( 'NONE', *, *, #1151, .T. ) ;
#16201 = DIRECTION ( 'NONE',  ( -0.06298685227120542907, -0.9980143568310855251, 1.515824502950130739E-13 ) ) ;
#16202 = CARTESIAN_POINT ( 'NONE',  ( -5.316799939240000938, 0.9999999999989999111, -150.0552959529999839 ) ) ;
#16203 = ORIENTED_EDGE ( 'NONE', *, *, #7015, .F. ) ;
#16204 = EDGE_CURVE ( 'NONE', #3040, #6070, #14549, .T. ) ;
#16205 = CIRCLE ( 'NONE', #6324, 8.176568160360000448 ) ;
#16206 = VECTOR ( 'NONE', #3861, 1000.000000000000000 ) ;
#16207 = CARTESIAN_POINT ( 'NONE',  ( -18.35824191589999899, -34.50000000000000000, -146.3157682190000060 ) ) ;
#16208 = ORIENTED_EDGE ( 'NONE', *, *, #195, .F. ) ;
#16209 = CARTESIAN_POINT ( 'NONE',  ( -15.50000000000000000, 47.50000000000000000, -137.0552959530000123 ) ) ;
#16210 = DIRECTION ( 'NONE',  ( 1.000000000000000000, 0.000000000000000000, 0.000000000000000000 ) ) ;
#16211 = LINE ( 'NONE', #21454, #1039 ) ;
#16212 = CARTESIAN_POINT ( 'NONE',  ( 7.477458949725431125, 38.09749598883478683, -141.8090149951282797 ) ) ;
#16213 = ORIENTED_EDGE ( 'NONE', *, *, #17582, .F. ) ;
#16214 = EDGE_CURVE ( 'NONE', #2750, #15988, #10850, .T. ) ;
#16215 = CARTESIAN_POINT ( 'NONE',  ( -18.11332094088754729, 35.20436099510112626, -148.1391246873896534 ) ) ;
#16216 = CARTESIAN_POINT ( 'NONE',  ( -8.245186567769970054, 40.93572612369973029, -144.5056815551646139 ) ) ;
#16217 = FACE_OUTER_BOUND ( 'NONE', #12565, .T. ) ;
#16218 = ORIENTED_EDGE ( 'NONE', *, *, #12136, .F. ) ;
#16219 = CARTESIAN_POINT ( 'NONE',  ( 20.50000000000000000, 25.50000000000000000, -136.0552959530000123 ) ) ;
#16220 = SURFACE_STYLE_USAGE ( .BOTH. , #713 ) ;
#16221 = ADVANCED_FACE ( 'NONE', ( #2059 ), #11912, .F. ) ;
#16222 = ORIENTED_EDGE ( 'NONE', *, *, #14324, .F. ) ;
#16223 = AXIS2_PLACEMENT_3D ( 'NONE', #16360, #21603, #21486 ) ;
#16224 = CARTESIAN_POINT ( 'NONE',  ( 5.792747474879999636, -16.92794981449999980, -145.5552959529999839 ) ) ;
#16225 = DIRECTION ( 'NONE',  ( -1.000000000000000000, 0.000000000000000000, -2.516505522483685870E-12 ) ) ;
#16226 = LINE ( 'NONE', #51, #8882 ) ;
#16227 = EDGE_CURVE ( 'NONE', #16611, #21713, #612, .T. ) ;
#16228 = EDGE_LOOP ( 'NONE', ( #17050, #3311, #8406 ) ) ;
#16229 = PLANE ( 'NONE',  #18249 ) ;
#16230 = PLANE ( 'NONE',  #4179 ) ;
#16231 = ORIENTED_EDGE ( 'NONE', *, *, #1613, .T. ) ;
#16232 = DIRECTION ( 'NONE',  ( -0.9848077530125620704, 4.409131086918041429E-28, -0.1736481776649230480 ) ) ;
#16233 = EDGE_CURVE ( 'NONE', #21733, #16939, #13093, .T. ) ;
#16234 = FACE_OUTER_BOUND ( 'NONE', #7565, .T. ) ;
#16235 = EDGE_CURVE ( 'NONE', #5378, #12200, #2518, .T. ) ;
#16236 = CARTESIAN_POINT ( 'NONE',  ( -16.50000000000000000, -43.00000000000000000, -140.0552959529999839 ) ) ;
#16237 = DIRECTION ( 'NONE',  ( 2.842170943040000002E-14, 3.570477247189999985E-13, 1.000000000000000000 ) ) ;
#16238 = EDGE_CURVE ( 'NONE', #11906, #3138, #6304, .T. ) ;
#16239 = VECTOR ( 'NONE', #20417, 1000.000000000000000 ) ;
#16240 = LINE ( 'NONE', #3510, #18847 ) ;
#16241 = EDGE_CURVE ( 'NONE', #4592, #21084, #10442, .T. ) ;
#16242 = VECTOR ( 'NONE', #18460, 1000.000000000000000 ) ;
#16243 = DIRECTION ( 'NONE',  ( -2.507771768023035002E-12, -1.592654560756634986E-17, 1.000000000000000000 ) ) ;
#16244 = ITEM_DEFINED_TRANSFORMATION ( 'NONE', 'NONE', #146,  #5025 ) ;
#16245 = DIRECTION ( 'NONE',  ( 1.000000000000000000, 0.000000000000000000, -2.257453483404485639E-12 ) ) ;
#16246 = CARTESIAN_POINT ( 'NONE',  ( -12.50000000000000000, 22.50000000000000000, -137.0552959530000123 ) ) ;
#16247 = CARTESIAN_POINT ( 'NONE',  ( -2.499999999940000439, 31.50000000000000000, -144.0552959529999839 ) ) ;
#16248 = VERTEX_POINT ( 'NONE', #4403 ) ;
#16249 = ORIENTED_EDGE ( 'NONE', *, *, #11919, .F. ) ;
#16250 = ORIENTED_EDGE ( 'NONE', *, *, #15036, .T. ) ;
#16251 = CARTESIAN_POINT ( 'NONE',  ( -4.499999999919999105, 34.00000000000000000, -135.0552959530000123 ) ) ;
#16252 = CARTESIAN_POINT ( 'NONE',  ( 21.39890631740000160, -21.26106171180000359, -145.0552959529999839 ) ) ;
#16253 = EDGE_LOOP ( 'NONE', ( #1668, #8678, #7432, #16394 ) ) ;
#16254 = DIRECTION ( 'NONE',  ( -2.256967945870000144E-12, 0.000000000000000000, -1.000000000000000000 ) ) ;
#16255 = VECTOR ( 'NONE', #3479, 999.9999999999998863 ) ;
#16256 = VERTEX_POINT ( 'NONE', #13330 ) ;
#16257 = DIRECTION ( 'NONE',  ( 2.257157423930000049E-12, 0.000000000000000000, 1.000000000000000000 ) ) ;
#16258 = CARTESIAN_POINT ( 'NONE',  ( 5.938276615700000427, -0.8672523143300000514, -135.0552959530000123 ) ) ;
#16259 = VECTOR ( 'NONE', #15824, 1000.000000000000000 ) ;
#16260 = PLANE ( 'NONE',  #16068 ) ;
#16261 = DIRECTION ( 'NONE',  ( -0.7633862853691524286, 0.6459422414661293299, -2.747801985950551593E-15 ) ) ;
#16262 = VERTEX_POINT ( 'NONE', #13207 ) ;
#16263 = CARTESIAN_POINT ( 'NONE',  ( 14.50000000010000001, 39.50000000000000000, -144.0552959529999839 ) ) ;
#16264 = ORIENTED_EDGE ( 'NONE', *, *, #18400, .T. ) ;
#16265 = CARTESIAN_POINT ( 'NONE',  ( 8.787969351399857132, 35.52785605379246903, -142.0347430632536714 ) ) ;
#16266 = EDGE_CURVE ( 'NONE', #21497, #20668, #20481, .T. ) ;
#16267 = DIRECTION ( 'NONE',  ( 0.000000000000000000, 0.000000000000000000, 1.000000000000000000 ) ) ;
#16268 = DIRECTION ( 'NONE',  ( 1.000000000000000000, 2.602084704489999637E-17, -1.701177084980000217E-20 ) ) ;
#16269 = EDGE_LOOP ( 'NONE', ( #425, #2875, #14130, #12103 ) ) ;
#16270 = CIRCLE ( 'NONE', #2212, 1.499999999999998446 ) ;
#16271 = DIRECTION ( 'NONE',  ( 0.000000000000000000, 0.000000000000000000, 1.000000000000000000 ) ) ;
#16272 = AXIS2_PLACEMENT_3D ( 'NONE', #17314, #13390, #13623 ) ;
#16273 = VERTEX_POINT ( 'NONE', #5837 ) ;
#16274 = LINE ( 'NONE', #14009, #1096 ) ;
#16275 = LINE ( 'NONE', #8760, #17313 ) ;
#16276 = EDGE_LOOP ( 'NONE', ( #15242, #7843, #18487, #21035 ) ) ;
#16277 = LINE ( 'NONE', #12102, #10328 ) ;
#16278 = ORIENTED_EDGE ( 'NONE', *, *, #7368, .T. ) ;
#16279 = CARTESIAN_POINT ( 'NONE',  ( -21.05404274330185288, 36.02007484894763678, -148.3253262703269399 ) ) ;
#16280 = CARTESIAN_POINT ( 'NONE',  ( -29.47785954729999958, 39.65718555499999809, -141.4786507110000287 ) ) ;
#16281 = ORIENTED_EDGE ( 'NONE', *, *, #14411, .F. ) ;
#16282 = DIRECTION ( 'NONE',  ( 0.000000000000000000, 0.000000000000000000, 1.000000000000000000 ) ) ;
#16283 = VERTEX_POINT ( 'NONE', #2170 ) ;
#16284 = CARTESIAN_POINT ( 'NONE',  ( 16.26858689138171243, -22.56086829267852778, -144.5552959530247108 ) ) ;
#16285 = ORIENTED_EDGE ( 'NONE', *, *, #10435, .T. ) ;
#16286 = EDGE_CURVE ( 'NONE', #896, #9140, #18055, .T. ) ;
#16287 = LINE ( 'NONE', #8649, #9106 ) ;
#16288 = DIRECTION ( 'NONE',  ( 0.1435602414469281940, 0.9896415801065048257, -3.836930773098079160E-13 ) ) ;
#16289 = AXIS2_PLACEMENT_3D ( 'NONE', #13939, #15488, #19298 ) ;
#16290 = ADVANCED_FACE ( 'NONE', ( #4299 ), #4060, .T. ) ;
#16291 = CARTESIAN_POINT ( 'NONE',  ( -30.99999999989999822, 37.00000000000000000, -139.0552959529999839 ) ) ;
#16292 = ORIENTED_EDGE ( 'NONE', *, *, #1766, .F. ) ;
#16293 = VECTOR ( 'NONE', #19767, 1000.000000000000000 ) ;
#16294 = CARTESIAN_POINT ( 'NONE',  ( -14.11967125440000004, 36.98834135279999913, -140.5455248810000057 ) ) ;
#16295 = CARTESIAN_POINT ( 'NONE',  ( -28.99249306591901032, 33.68760113747161000, -142.1526180105009871 ) ) ;
#16296 = VECTOR ( 'NONE', #14265, 1000.000000000000114 ) ;
#16297 = ORIENTED_EDGE ( 'NONE', *, *, #22197, .T. ) ;
#16298 = CARTESIAN_POINT ( 'NONE',  ( -30.49999999990000177, 29.00000000000000000, -140.5552959529999839 ) ) ;
#16299 = CARTESIAN_POINT ( 'NONE',  ( 3.000000000000000000, -3.500000000000000000, -150.0552959529999839 ) ) ;
#16300 = CARTESIAN_POINT ( 'NONE',  ( -17.42663577349999926, 38.80963643279999786, -139.8270276149999916 ) ) ;
#16301 = LINE ( 'NONE', #6, #17847 ) ;
#16302 = ORIENTED_EDGE ( 'NONE', *, *, #17107, .F. ) ;
#16303 = CARTESIAN_POINT ( 'NONE',  ( 5.519360106986514580, 13.04803137664692336, -136.0552959530124895 ) ) ;
#16304 = PLANE ( 'NONE',  #9705 ) ;
#16305 = PLANE ( 'NONE',  #14081 ) ;
#16306 = CARTESIAN_POINT ( 'NONE',  ( -6.657076963140000636, -20.13603737529999904, -144.5552959529999839 ) ) ;
#16307 = CARTESIAN_POINT ( 'NONE',  ( -35.47299999999999898, 16.95803989150000035, -143.5552959529999839 ) ) ;
#16308 = CARTESIAN_POINT ( 'NONE',  ( 15.97954986339999905, -26.72957102550000030, -142.5552959529999839 ) ) ;
#16309 = EDGE_LOOP ( 'NONE', ( #4245, #19345, #16112, #4902 ) ) ;
#16310 = CARTESIAN_POINT ( 'NONE',  ( -31.50000000000000000, -50.00000000000000000, -137.0552959530000123 ) ) ;
#16311 = CARTESIAN_POINT ( 'NONE',  ( -14.07987191918735270, -41.79896944934834124, -136.0552959529682084 ) ) ;
#16312 = AXIS2_PLACEMENT_3D ( 'NONE', #16703, #5760, #22186 ) ;
#16313 = DIRECTION ( 'NONE',  ( 0.000000000000000000, -2.257144641399999941E-12, 1.000000000000000000 ) ) ;
#16314 = CARTESIAN_POINT ( 'NONE',  ( -5.642215125958555788, 41.80899724057998412, -143.5028856654435003 ) ) ;
#16315 = LINE ( 'NONE', #1584, #14050 ) ;
#16316 = EDGE_LOOP ( 'NONE', ( #5762, #20597, #22842, #19112 ) ) ;
#16317 = EDGE_CURVE ( 'NONE', #1507, #10304, #9391, .T. ) ;
#16318 = CARTESIAN_POINT ( 'NONE',  ( 10.06934556926865376, -21.30022032142531430, -148.5552959529999839 ) ) ;
#16319 = CARTESIAN_POINT ( 'NONE',  ( 8.995627988029999855, -17.23072307649999857, -146.0552959529999839 ) ) ;
#16320 = EDGE_CURVE ( 'NONE', #21917, #2716, #21871, .T. ) ;
#16321 = VERTEX_POINT ( 'NONE', #17137 ) ;
#16322 = AXIS2_PLACEMENT_3D ( 'NONE', #11792, #995, #4675 ) ;
#16323 = AXIS2_PLACEMENT_3D ( 'NONE', #10688, #3327, #17849 ) ;
#16324 = DIRECTION ( 'NONE',  ( 1.000000000000000000, -5.094701932209999624E-24, -2.257144641399999941E-12 ) ) ;
#16325 = EDGE_LOOP ( 'NONE', ( #8973, #5265, #18947, #11828 ) ) ;
#16326 = VECTOR ( 'NONE', #11487, 1000.000000000000000 ) ;
#16327 = CARTESIAN_POINT ( 'NONE',  ( 32.50000000000000000, 39.92025131100000124, -150.0552959529999839 ) ) ;
#16328 = CARTESIAN_POINT ( 'NONE',  ( -30.45874311816843516, 41.26340968600602110, -144.2604718650849520 ) ) ;
#16329 = AXIS2_PLACEMENT_3D ( 'NONE', #21395, #12562, #8871 ) ;
#16330 = CARTESIAN_POINT ( 'NONE',  ( -21.23917607309999767, 35.28761490579999816, -147.7082871199999943 ) ) ;
#16331 = CARTESIAN_POINT ( 'NONE',  ( 7.135907599097732756, 36.37446523411252741, -141.6344350119672981 ) ) ;
#16332 = VERTEX_POINT ( 'NONE', #2295 ) ;
#16333 = LINE ( 'NONE', #7284, #1814 ) ;
#16334 = CARTESIAN_POINT ( 'NONE',  ( -19.28863050619207087, 36.17828169457454379, -139.9441849802047955 ) ) ;
#16335 = CARTESIAN_POINT ( 'NONE',  ( -18.35824191589999899, -13.50000000000000000, -144.8157682190000060 ) ) ;
#16336 = LINE ( 'NONE', #3361, #22866 ) ;
#16337 = ORIENTED_EDGE ( 'NONE', *, *, #9256, .F. ) ;
#16338 = DIRECTION ( 'NONE',  ( -1.000000000000000000, 0.000000000000000000, 0.000000000000000000 ) ) ;
#16339 = EDGE_CURVE ( 'NONE', #19299, #11584, #16788, .T. ) ;
#16340 = ORIENTED_EDGE ( 'NONE', *, *, #8654, .T. ) ;
#16341 = DIRECTION ( 'NONE',  ( 0.000000000000000000, -1.000000000000000000, 3.568879590630000244E-13 ) ) ;
#16342 = CARTESIAN_POINT ( 'NONE',  ( 1.133692148650000009, 50.50000000000000000, -136.0552959530000123 ) ) ;
#16343 = CARTESIAN_POINT ( 'NONE',  ( -4.576509874723263316, 21.71905350741257834, -136.0552959529896384 ) ) ;
#16344 = AXIS2_PLACEMENT_3D ( 'NONE', #22196, #5883, #17186 ) ;
#16345 = CIRCLE ( 'NONE', #6077, 5.000000000000000000 ) ;
#16346 = ORIENTED_EDGE ( 'NONE', *, *, #23218, .F. ) ;
#16347 = AXIS2_PLACEMENT_3D ( 'NONE', #9836, #7825, #9958 ) ;
#16348 = DIRECTION ( 'NONE',  ( 2.602084747549999882E-17, -1.000000000000000000, -5.873289694040000105E-29 ) ) ;
#16349 = VECTOR ( 'NONE', #6647, 1000.000000000000000 ) ;
#16350 = DIRECTION ( 'NONE',  ( 0.000000000000000000, 0.000000000000000000, 1.000000000000000000 ) ) ;
#16351 = ADVANCED_FACE ( 'NONE', ( #2410 ), #9627, .F. ) ;
#16352 = VERTEX_POINT ( 'NONE', #19040 ) ;
#16353 = CARTESIAN_POINT ( 'NONE',  ( -17.44989882389999991, 40.67283837529999602, -143.6255418399999826 ) ) ;
#16354 = DIRECTION ( 'NONE',  ( 1.000000000000000000, 0.000000000000000000, -8.955190032050000935E-12 ) ) ;
#16355 = CARTESIAN_POINT ( 'NONE',  ( -14.24283201953359956, -44.30969209386396557, -150.0552959529999839 ) ) ;
#16356 = LINE ( 'NONE', #16466, #14831 ) ;
#16357 = CARTESIAN_POINT ( 'NONE',  ( 23.08797222880000177, -15.45109671570000032, -142.5552959529999839 ) ) ;
#16358 = ADVANCED_FACE ( 'NONE', ( #13684 ), #1085, .T. ) ;
#16359 = CARTESIAN_POINT ( 'NONE',  ( 14.71940181155087579, 39.42378041200768735, -150.0552959530000123 ) ) ;
#16360 = CARTESIAN_POINT ( 'NONE',  ( 19.34345092960000301, -49.66753540199999151, -149.5552959529999839 ) ) ;
#16361 = CARTESIAN_POINT ( 'NONE',  ( 1.133692148550000001, 50.50000000000000000, -137.0552959530000123 ) ) ;
#16362 = AXIS2_PLACEMENT_3D ( 'NONE', #15759, #15867, #23021 ) ;
#16363 = CARTESIAN_POINT ( 'NONE',  ( 6.500000000040000003, 28.00000000000000000, -136.0552959530000123 ) ) ;
#16364 = ORIENTED_EDGE ( 'NONE', *, *, #22038, .F. ) ;
#16365 = UNCERTAINTY_MEASURE_WITH_UNIT (LENGTH_MEASURE( 1.000000000000000082E-05 ), #10401, 'distance_accuracy_value', 'NONE');
#16366 = VERTEX_POINT ( 'NONE', #21423 ) ;
#16367 = EDGE_CURVE ( 'NONE', #19736, #4115, #6542, .T. ) ;
#16368 = EDGE_CURVE ( 'NONE', #14626, #2447, #12008, .T. ) ;
#16369 = ORIENTED_EDGE ( 'NONE', *, *, #10787, .F. ) ;
#16370 = CARTESIAN_POINT ( 'NONE',  ( -32.50000000000000000, 12.08229784559999942, -147.5656262009999864 ) ) ;
#16371 = DIRECTION ( 'NONE',  ( -1.211690350419999855E-27, -2.765629237170000203E-27, 1.000000000000000000 ) ) ;
#16372 = CARTESIAN_POINT ( 'NONE',  ( -4.888913597060000171, -24.24628707910000003, -143.5552959529999839 ) ) ;
#16373 = CARTESIAN_POINT ( 'NONE',  ( -4.499999999939999995, 42.50000000000000000, -144.0552959529999839 ) ) ;
#16374 = ADVANCED_FACE ( 'NONE', ( #8440, #17723, #6892 ), #15940, .T. ) ;
#16375 = EDGE_LOOP ( 'NONE', ( #20739, #9519, #3722, #19456 ) ) ;
#16376 = CARTESIAN_POINT ( 'NONE',  ( -5.985376956606384802, 25.11919234682651236, -150.0552959530000123 ) ) ;
#16377 = ADVANCED_FACE ( 'NONE', ( #3102 ), #8658, .T. ) ;
#16378 = CARTESIAN_POINT ( 'NONE',  ( -20.30489103444976351, 34.41680263911344895, -140.8326631860697091 ) ) ;
#16379 = DIRECTION ( 'NONE',  ( 1.526468026909999897E-13, 8.159623473500000156E-13, 1.000000000000000000 ) ) ;
#16380 = CARTESIAN_POINT ( 'NONE',  ( -32.50000000000000000, 51.00000000000000000, -149.5552959529999839 ) ) ;
#16381 = ORIENTED_EDGE ( 'NONE', *, *, #13015, .F. ) ;
#16382 = DIRECTION ( 'NONE',  ( 0.000000000000000000, 3.900299903225544950E-11, -1.000000000000000000 ) ) ;
#16383 = EDGE_LOOP ( 'NONE', ( #14191, #5989 ) ) ;
#16384 = CARTESIAN_POINT ( 'NONE',  ( 9.057761017886996058, 35.60753996401869159, -141.9790531660381703 ) ) ;
#16385 = DIRECTION ( 'NONE',  ( 2.257749542879999954E-12, 0.000000000000000000, 1.000000000000000000 ) ) ;
#16386 = LINE ( 'NONE', #3297, #15563 ) ;
#16387 = VERTEX_POINT ( 'NONE', #1437 ) ;
#16388 = CARTESIAN_POINT ( 'NONE',  ( -31.75000000000000000, 1.000000000000000000, -151.0552959529999839 ) ) ;
#16389 = ORIENTED_EDGE ( 'NONE', *, *, #21188, .T. ) ;
#16390 = CARTESIAN_POINT ( 'NONE',  ( 5.148789539621256850, -48.22641955295573268, -150.0552959529999839 ) ) ;
#16391 = CIRCLE ( 'NONE', #8759, 0.4999999999999987788 ) ;
#16392 = LINE ( 'NONE', #103, #21527 ) ;
#16393 =( GEOMETRIC_REPRESENTATION_CONTEXT ( 3 ) GLOBAL_UNCERTAINTY_ASSIGNED_CONTEXT ( ( #14226 ) ) GLOBAL_UNIT_ASSIGNED_CONTEXT ( ( #23332, #16648, #248 ) ) REPRESENTATION_CONTEXT ( 'NONE', 'WORKASPACE' ) );
#16394 = ORIENTED_EDGE ( 'NONE', *, *, #6416, .F. ) ;
#16395 = CARTESIAN_POINT ( 'NONE',  ( -26.86882954950000268, 40.29793777999999804, -142.0811670120000088 ) ) ;
#16396 = EDGE_CURVE ( 'NONE', #12941, #14758, #6654, .T. ) ;
#16397 = ORIENTED_EDGE ( 'NONE', *, *, #9731, .T. ) ;
#16398 = CARTESIAN_POINT ( 'NONE',  ( -15.86078924153199310, 37.04043998683727779, -147.5134597624270612 ) ) ;
#16399 = EDGE_CURVE ( 'NONE', #20106, #19898, #965, .T. ) ;
#16400 = DIRECTION ( 'NONE',  ( 2.602084704489999637E-17, -1.000000000000000000, -4.426606872070000353E-37 ) ) ;
#16401 = ORIENTED_EDGE ( 'NONE', *, *, #14618, .T. ) ;
#16402 = PRODUCT_CONTEXT ( 'NONE', #2653, 'mechanical' ) ;
#16403 = ORIENTED_EDGE ( 'NONE', *, *, #21347, .F. ) ;
#16404 = DIRECTION ( 'NONE',  ( -0.9753087663813413410, 0.2208456705930775810, 8.935806277123132252E-12 ) ) ;
#16405 = LINE ( 'NONE', #3558, #3895 ) ;
#16406 = DIRECTION ( 'NONE',  ( 0.000000000000000000, 4.426606872070000353E-37, -1.000000000000000000 ) ) ;
#16407 = CARTESIAN_POINT ( 'NONE',  ( -9.282104535860000283, -16.71402168319999859, -145.5552959529999839 ) ) ;
#16408 = DIRECTION ( 'NONE',  ( 1.000000000000000000, 0.000000000000000000, -2.253619677469999738E-12 ) ) ;
#16409 = ORIENTED_EDGE ( 'NONE', *, *, #13561, .F. ) ;
#16410 = CARTESIAN_POINT ( 'NONE',  ( -15.46613156839999981, 36.99333119719999985, -147.5584717940000132 ) ) ;
#16411 = VECTOR ( 'NONE', #17977, 1000.000000000000000 ) ;
#16412 = AXIS2_PLACEMENT_3D ( 'NONE', #9429, #18619, #15162 ) ;
#16413 = CIRCLE ( 'NONE', #11462, 8.176568160360000448 ) ;
#16414 = LINE ( 'NONE', #2376, #1141 ) ;
#16415 = ORIENTED_EDGE ( 'NONE', *, *, #20551, .T. ) ;
#16416 = LINE ( 'NONE', #20337, #1794 ) ;
#16417 = CARTESIAN_POINT ( 'NONE',  ( -21.35824191589999899, -4.750000000000000000, -146.3157682190075093 ) ) ;
#16418 = CARTESIAN_POINT ( 'NONE',  ( -17.06385656868887324, 41.33018260709537373, -143.5869266124798855 ) ) ;
#16419 = CARTESIAN_POINT ( 'NONE',  ( -5.070907855439999778, -22.41528233759999722, -148.0552959529999839 ) ) ;
#16420 = VERTEX_POINT ( 'NONE', #10218 ) ;
#16421 = CARTESIAN_POINT ( 'NONE',  ( -0.2408409771846180825, 17.17512194927200397, -136.0552959529995007 ) ) ;
#16422 = LINE ( 'NONE', #7374, #19995 ) ;
#16423 = DIRECTION ( 'NONE',  ( -0.3989061605089001539, -0.7301928289268172501, 0.5547001962248612195 ) ) ;
#16424 = DIRECTION ( 'NONE',  ( 0.000000000000000000, 0.000000000000000000, 1.000000000000000000 ) ) ;
#16425 = CARTESIAN_POINT ( 'NONE',  ( -6.601136089949999786, -20.10368962670000315, -143.5552959529999839 ) ) ;
#16426 = EDGE_CURVE ( 'NONE', #19021, #17769, #13918, .T. ) ;
#16427 = DIRECTION ( 'NONE',  ( 1.000000000000000000, 0.000000000000000000, 0.000000000000000000 ) ) ;
#16428 = EDGE_CURVE ( 'NONE', #11114, #4660, #19856, .T. ) ;
#16429 = CIRCLE ( 'NONE', #7302, 35.00000000000000000 ) ;
#16430 = EDGE_LOOP ( 'NONE', ( #4009, #113, #2969, #5065 ) ) ;
#16431 = CIRCLE ( 'NONE', #118, 8.176568160360000448 ) ;
#16432 = LINE ( 'NONE', #10573, #1971 ) ;
#16433 = LINE ( 'NONE', #139, #4963 ) ;
#16434 = DIRECTION ( 'NONE',  ( 1.000000000000000000, 0.000000000000000000, -2.257144641399999941E-12 ) ) ;
#16435 = CARTESIAN_POINT ( 'NONE',  ( -6.356911216211141635, 38.98543411609163911, -148.4775420273327597 ) ) ;
#16436 = DIRECTION ( 'NONE',  ( -0.1146332952500066227, -0.9934078757590583120, -9.710750722050572275E-14 ) ) ;
#16437 = B_SPLINE_CURVE_WITH_KNOTS ( 'NONE', 3,
 ( #22320, #4116, #2351, #5666, #13043, #9111, #16728, #5555, #20542, #6014, #319, #14949, #204, #16390, #22209, #12801, #7343, #2230 ),
 .UNSPECIFIED., .F., .F.,
 ( 4, 2, 2, 2, 2, 2, 2, 2, 4 ),
 ( 0.000000000000000000, 0.1250000000000000000, 0.2500000000000000000, 0.3750000000000000000, 0.5000000000000000000, 0.6250000000000000000, 0.7500000000000000000, 0.8750000000000000000, 1.000000000000000000 ),
 .UNSPECIFIED. ) ;
#16438 = ORIENTED_EDGE ( 'NONE', *, *, #2842, .F. ) ;
#16439 = CARTESIAN_POINT ( 'NONE',  ( -2.718705559363074897, -28.41053430194196494, -145.5552959530122905 ) ) ;
#16440 = FACE_OUTER_BOUND ( 'NONE', #2925, .T. ) ;
#16441 = VERTEX_POINT ( 'NONE', #9980 ) ;
#16442 = ORIENTED_EDGE ( 'NONE', *, *, #354, .F. ) ;
#16443 = AXIS2_PLACEMENT_3D ( 'NONE', #22683, #13636, #4364 ) ;
#16444 = CARTESIAN_POINT ( 'NONE',  ( -23.48449349015690046, 36.94479390616788095, -140.4349842069357521 ) ) ;
#16445 = CARTESIAN_POINT ( 'NONE',  ( -30.03413168677343492, 40.19007108948994045, -140.8797962025610104 ) ) ;
#16446 = CARTESIAN_POINT ( 'NONE',  ( -15.90886514219999981, -34.50000000000000000, -148.5657682190000060 ) ) ;
#16447 = LINE ( 'NONE', #1949, #22790 ) ;
#16448 = EDGE_LOOP ( 'NONE', ( #14147, #5856, #23459, #18398 ) ) ;
#16449 = CARTESIAN_POINT ( 'NONE',  ( -19.28609856413475754, 34.66429844331295840, -140.9609051183012127 ) ) ;
#16450 = FACE_OUTER_BOUND ( 'NONE', #16383, .T. ) ;
#16451 = CARTESIAN_POINT ( 'NONE',  ( 9.660841442712255756, -32.96298433614438039, -136.0552959530218118 ) ) ;
#16452 = ADVANCED_FACE ( 'NONE', ( #1324 ), #23085, .T. ) ;
#16453 = CARTESIAN_POINT ( 'NONE',  ( -23.02245220108656909, 38.00600600913553961, -139.3782448799144618 ) ) ;
#16454 = EDGE_CURVE ( 'NONE', #7907, #15538, #21307, .T. ) ;
#16455 = CARTESIAN_POINT ( 'NONE',  ( 6.500000000000000000, 20.50000000000000000, -151.0552959529999839 ) ) ;
#16456 = DIRECTION ( 'NONE',  ( -0.1000233216789610108, -0.9949850929136109245, 3.591470555298595137E-13 ) ) ;
#16457 = LINE ( 'NONE', #9404, #11831 ) ;
#16458 = COLOUR_RGB ( '', 0.40784314, 0.44705882, 0.49803922) ;
#16459 = LINE ( 'NONE', #3848, #19926 ) ;
#16460 = ORIENTED_EDGE ( 'NONE', *, *, #14141, .T. ) ;
#16461 = CARTESIAN_POINT ( 'NONE',  ( -6.807579269534479671, 38.78453684425459613, -147.8970667730299908 ) ) ;
#16462 = VERTEX_POINT ( 'NONE', #12242 ) ;
#16463 = CARTESIAN_POINT ( 'NONE',  ( 1.133692148650000009, 51.50000000000000000, -136.5552959530000123 ) ) ;
#16464 = CARTESIAN_POINT ( 'NONE',  ( -25.86630785139999844, -51.00000000000000000, -136.0552959530000123 ) ) ;
#16465 = LINE ( 'NONE', #3856, #15054 ) ;
#16466 = CARTESIAN_POINT ( 'NONE',  ( 31.64594224149999846, -40.56768785850000825, -150.0552959529999839 ) ) ;
#16467 = DIRECTION ( 'NONE',  ( 0.000000000000000000, 2.256988247090000272E-12, 1.000000000000000000 ) ) ;
#16468 = CARTESIAN_POINT ( 'NONE',  ( -20.60824191589999899, -32.00000000000000000, -144.8157682190000060 ) ) ;
#16469 = DIRECTION ( 'NONE',  ( 0.000000000000000000, 0.000000000000000000, 1.000000000000000000 ) ) ;
#16470 = AXIS2_PLACEMENT_3D ( 'NONE', #8767, #16282, #1546 ) ;
#16471 = DIRECTION ( 'NONE',  ( 0.000000000000000000, 0.000000000000000000, -1.000000000000000000 ) ) ;
#16472 = CARTESIAN_POINT ( 'NONE',  ( -13.40552595227777211, 37.07358616897466419, -140.3498584192782062 ) ) ;
#16473 =( REPRESENTATION_RELATIONSHIP ('NONE','NONE', #7672, #14082 ) REPRESENTATION_RELATIONSHIP_WITH_TRANSFORMATION ( #19577 )SHAPE_REPRESENTATION_RELATIONSHIP( ) );
#16474 = EDGE_LOOP ( 'NONE', ( #7773, #21747, #19243, #20499 ) ) ;
#16475 = ADVANCED_FACE ( 'NONE', ( #2863 ), #19520, .F. ) ;
#16476 = ORIENTED_EDGE ( 'NONE', *, *, #18049, .F. ) ;
#16477 = VERTEX_POINT ( 'NONE', #17257 ) ;
#16478 = CARTESIAN_POINT ( 'NONE',  ( -16.63107678121195931, 35.60580843633908188, -140.6802342586736074 ) ) ;
#16479 = CARTESIAN_POINT ( 'NONE',  ( -12.76385253868072134, 37.02886902027827887, -147.6186336933980101 ) ) ;
#16480 = ORIENTED_EDGE ( 'NONE', *, *, #18197, .T. ) ;
#16481 = CARTESIAN_POINT ( 'NONE',  ( 7.750000000030000002, -37.98606797749999942, -136.0552959530000123 ) ) ;
#16482 = ORIENTED_EDGE ( 'NONE', *, *, #2853, .F. ) ;
#16483 = CARTESIAN_POINT ( 'NONE',  ( 25.50006728700737924, 36.10251055750465099, -136.0552959530575663 ) ) ;
#16484 = EDGE_CURVE ( 'NONE', #12948, #5167, #13810, .T. ) ;
#16485 = CARTESIAN_POINT ( 'NONE',  ( -19.79211671321127497, 32.85031535814157166, -144.7688754269952938 ) ) ;
#16486 = CARTESIAN_POINT ( 'NONE',  ( -17.01442029460000072, -34.50000000000000000, -147.5657682190000060 ) ) ;
#16487 = EDGE_LOOP ( 'NONE', ( #8878, #10555, #11549, #10606 ) ) ;
#16488 = LINE ( 'NONE', #21746, #11414 ) ;
#16489 = CARTESIAN_POINT ( 'NONE',  ( 8.500000000060001781, 38.50000000000000000, -142.0552959529999839 ) ) ;
#16490 = EDGE_CURVE ( 'NONE', #16855, #9023, #7130, .T. ) ;
#16491 = DIRECTION ( 'NONE',  ( 2.257157423930000049E-12, 0.000000000000000000, 1.000000000000000000 ) ) ;
#16492 = LINE ( 'NONE', #21971, #12042 ) ;
#16493 = ORIENTED_EDGE ( 'NONE', *, *, #6385, .F. ) ;
#16494 = EDGE_CURVE ( 'NONE', #4645, #22981, #5578, .T. ) ;
#16495 = DIRECTION ( 'NONE',  ( -0.7633862853691524286, 0.6459422414661293299, 0.000000000000000000 ) ) ;
#16496 = ORIENTED_EDGE ( 'NONE', *, *, #22317, .T. ) ;
#16497 = LINE ( 'NONE', #7448, #23488 ) ;
#16498 = ORIENTED_EDGE ( 'NONE', *, *, #20586, .F. ) ;
#16499 = CARTESIAN_POINT ( 'NONE',  ( -26.08236470951569785, 39.06228944650155199, -141.2475209953871342 ) ) ;
#16500 = ORIENTED_EDGE ( 'NONE', *, *, #3145, .F. ) ;
#16501 = VECTOR ( 'NONE', #15163, 1000.000000000000000 ) ;
#16502 = CARTESIAN_POINT ( 'NONE',  ( -22.42941481613483745, 36.22509709915611609, -139.9955747715279983 ) ) ;
#16503 = ORIENTED_EDGE ( 'NONE', *, *, #17660, .T. ) ;
#16504 = FACE_OUTER_BOUND ( 'NONE', #17241, .T. ) ;
#16505 = VERTEX_POINT ( 'NONE', #16299 ) ;
#16506 = APPLICATION_PROTOCOL_DEFINITION ( 'draft international standard', 'automotive_design', 1998, #22556 ) ;
#16507 =( BOUNDED_SURFACE ( )  B_SPLINE_SURFACE ( 5, 5, ( 
 ( #4217, #15156, #5870, #2674, #22074, #22420 ),
 ( #9663, #6113, #20753, #11454, #4334, #14927 ),
 ( #17051, #9554, #4094, #11567, #13020, #18842 ),
 ( #6229, #14815, #18612, #13479, #539, #13129 ),
 ( #4446, #11682, #20401, #11328, #16829, #7771 ),
 ( #15034, #5988, #22298, #13244, #8464, #22992 ),
 ( #13942, #17396, #10470, #13833, #21096, #11791 ),
 ( #21214, #16295, #3013, #1114, #7249, #20856 ),
 ( #4904, #6679, #17516, #21334, #8570, #22752 ),
 ( #10251, #12153, #11914, #8686, #4553, #19424 ),
 ( #15732, #3129, #3236, #1237, #10360, #993 ),
 ( #23540, #17636, #1345, #4788, #19181, #15841 ) ),
 .UNSPECIFIED., .F., .F., .F. ) 
 B_SPLINE_SURFACE_WITH_KNOTS ( ( 6, 3, 3, 6 ),
 ( 6, 6 ),
 ( 0.000000000000000000, 4.564346237179999655, 9.066392868600001265, 13.51003987140000007 ),
 ( 0.000000000000000000, 1.570796326752264882 ),
 .UNSPECIFIED. ) 
 GEOMETRIC_REPRESENTATION_ITEM ( )  RATIONAL_B_SPLINE_SURFACE ( (
 ( 1.000000000000000000, 0.6000000000108819398, 0.4000000000108820397, 0.3000000000081615159, 0.2500000000054409810, 0.2500000000000000000),
 ( 1.000000000000000000, 0.6000000000108819398, 0.4000000000108820397, 0.3000000000081615159, 0.2500000000054409810, 0.2500000000000000000),
 ( 1.000000000000000000, 0.6000000000108819398, 0.4000000000108820397, 0.3000000000081615159, 0.2500000000054409810, 0.2500000000000000000),
 ( 1.000000000000000000, 0.6000000000108819398, 0.4000000000108820397, 0.3000000000081615159, 0.2500000000054409810, 0.2500000000000000000),
 ( 1.000000000000000000, 0.6000000000108819398, 0.4000000000108820397, 0.3000000000081615159, 0.2500000000054409810, 0.2500000000000000000),
 ( 1.000000000000000000, 0.6000000000108819398, 0.4000000000108820397, 0.3000000000081615159, 0.2500000000054409810, 0.2500000000000000000),
 ( 1.000000000000000000, 0.6000000000108819398, 0.4000000000108820397, 0.3000000000081615159, 0.2500000000054409810, 0.2500000000000000000),
 ( 1.000000000000000000, 0.6000000000108819398, 0.4000000000108820397, 0.3000000000081615159, 0.2500000000054409810, 0.2500000000000000000),
 ( 1.000000000000000000, 0.6000000000108819398, 0.4000000000108820397, 0.3000000000081615159, 0.2500000000054409810, 0.2500000000000000000),
 ( 1.000000000000000000, 0.6000000000108819398, 0.4000000000108820397, 0.3000000000081615159, 0.2500000000054409810, 0.2500000000000000000),
 ( 1.000000000000000000, 0.6000000000108819398, 0.4000000000108820397, 0.3000000000081615159, 0.2500000000054409810, 0.2500000000000000000),
 ( 1.000000000000000000, 0.6000000000108819398, 0.4000000000108820397, 0.3000000000081615159, 0.2500000000054409810, 0.2500000000000000000) ) ) 
 REPRESENTATION_ITEM ( '' )  SURFACE ( )  );
#16508 = VERTEX_POINT ( 'NONE', #8900 ) ;
#16509 = DIRECTION ( 'NONE',  ( 1.000000000000000000, 2.688820921349999492E-17, 0.000000000000000000 ) ) ;
#16510 = ADVANCED_FACE ( 'NONE', ( #9254 ), #14737, .F. ) ;
#16511 = CARTESIAN_POINT ( 'NONE',  ( 25.31684607429999900, 45.26810052439999765, -137.0552959530000123 ) ) ;
#16512 = CARTESIAN_POINT ( 'NONE',  ( 31.00000000000000000, 39.80430157320000006, -149.5552959529999839 ) ) ;
#16513 = LINE ( 'NONE', #14725, #13999 ) ;
#16514 = EDGE_CURVE ( 'NONE', #8221, #3481, #19629, .T. ) ;
#16515 = CARTESIAN_POINT ( 'NONE',  ( -10.59674732016127585, 36.36477667316268025, -140.6486635252139195 ) ) ;
#16516 = DIRECTION ( 'NONE',  ( -0.1465035852930155202, -0.9892101392001055871, 4.561368942930487546E-14 ) ) ;
#16517 = B_SPLINE_CURVE_WITH_KNOTS ( 'NONE', 3,
 ( #8204, #5005, #15472, #3110, #22731, #2990, #6430, #10226, #20963, #4654, #22862, #11895, #6549, #13816, #4768, #17497, #1219, #15714 ),
 .UNSPECIFIED., .F., .F.,
 ( 4, 2, 2, 2, 2, 2, 2, 2, 4 ),
 ( 0.000000000000000000, 0.1250000000000000000, 0.2500000000000000000, 0.3750000000000000000, 0.5000000000000000000, 0.6250000000000000000, 0.7500000000000000000, 0.8750000000000000000, 1.000000000000000000 ),
 .UNSPECIFIED. ) ;
#16518 = ORIENTED_EDGE ( 'NONE', *, *, #3159, .F. ) ;
#16519 = CARTESIAN_POINT ( 'NONE',  ( 18.18320006080000084, 0.4999999999990000776, -149.3052959529999839 ) ) ;
#16520 = ADVANCED_FACE ( 'NONE', ( #5471 ), #1791, .T. ) ;
#16521 = CARTESIAN_POINT ( 'NONE',  ( 8.986817037251329410, 35.58084844828771764, -146.1134792699400009 ) ) ;
#16522 = EDGE_CURVE ( 'NONE', #1779, #2894, #19983, .T. ) ;
#16523 = ORIENTED_EDGE ( 'NONE', *, *, #9977, .F. ) ;
#16524 = CARTESIAN_POINT ( 'NONE',  ( 8.500000000070000894, 37.00000000000000000, -138.5552959529999839 ) ) ;
#16525 = EDGE_CURVE ( 'NONE', #11605, #11936, #16526, .T. ) ;
#16526 = LINE ( 'NONE', #234, #13102 ) ;
#16527 = EDGE_CURVE ( 'NONE', #17890, #3657, #11447, .T. ) ;
#16528 = CARTESIAN_POINT ( 'NONE',  ( -18.09080689940000397, 41.54765954780000214, -144.4256796519999853 ) ) ;
#16529 = CARTESIAN_POINT ( 'NONE',  ( -22.52056272209999932, 33.27763168300000274, -146.2006519230000094 ) ) ;
#16530 = VERTEX_POINT ( 'NONE', #14519 ) ;
#16531 = LINE ( 'NONE', #238, #680 ) ;
#16532 = FACE_OUTER_BOUND ( 'NONE', #7379, .T. ) ;
#16533 = FACE_BOUND ( 'NONE', #15519, .T. ) ;
#16534 = DIRECTION ( 'NONE',  ( 0.000000000000000000, 1.000000000000000000, 0.000000000000000000 ) ) ;
#16535 = CARTESIAN_POINT ( 'NONE',  ( -17.22605506639999717, 36.97564272059999979, -139.5994799229999899 ) ) ;
#16536 = CARTESIAN_POINT ( 'NONE',  ( -15.46613156839999981, 36.99333119719999985, -147.5584717940000132 ) ) ;
#16537 = ORIENTED_EDGE ( 'NONE', *, *, #744, .T. ) ;
#16538 = CARTESIAN_POINT ( 'NONE',  ( -27.55423410434942255, 32.98668071434571658, -144.3507793926698071 ) ) ;
#16539 = LINE ( 'NONE', #22020, #4579 ) ;
#16540 = CARTESIAN_POINT ( 'NONE',  ( 32.50000000000000000, -40.03620104880000241, -149.5552959529999839 ) ) ;
#16541 = VECTOR ( 'NONE', #7369, 1000.000000000000000 ) ;
#16542 = CARTESIAN_POINT ( 'NONE',  ( -32.00000000000000000, 19.50000000000000000, -149.5552959529999839 ) ) ;
#16543 = DIRECTION ( 'NONE',  ( -1.000000000000000000, 0.000000000000000000, 2.257120985840000117E-12 ) ) ;
#16544 = EDGE_LOOP ( 'NONE', ( #4804, #13813, #8971 ) ) ;
#16545 = CARTESIAN_POINT ( 'NONE',  ( -27.04496201379999931, 40.71797592360000095, -143.5957174049999878 ) ) ;
#16546 = CARTESIAN_POINT ( 'NONE',  ( -34.50000000000000000, 0.9999999999959999775, -144.0552959529999839 ) ) ;
#16547 = ORIENTED_EDGE ( 'NONE', *, *, #1995, .F. ) ;
#16548 = EDGE_CURVE ( 'NONE', #5742, #473, #21786, .T. ) ;
#16549 = VERTEX_POINT ( 'NONE', #3683 ) ;
#16550 = CARTESIAN_POINT ( 'NONE',  ( 6.000000000010004442, -3.300767767050150070, -136.0552959530135411 ) ) ;
#16551 = LINE ( 'NONE', #18350, #23424 ) ;
#16552 = FACE_OUTER_BOUND ( 'NONE', #21525, .T. ) ;
#16553 = DIRECTION ( 'NONE',  ( 0.000000000000000000, 0.000000000000000000, -1.000000000000000000 ) ) ;
#16554 = VECTOR ( 'NONE', #7998, 1000.000000000000000 ) ;
#16555 = ORIENTED_EDGE ( 'NONE', *, *, #19127, .T. ) ;
#16556 = SURFACE_STYLE_FILL_AREA ( #11421 ) ;
#16557 = VECTOR ( 'NONE', #434, 1000.000000000000000 ) ;
#16558 = CARTESIAN_POINT ( 'NONE',  ( -18.42429559863251498, 33.08108273512412723, -146.4504986391189050 ) ) ;
#16559 = FACE_OUTER_BOUND ( 'NONE', #20313, .T. ) ;
#16560 = CARTESIAN_POINT ( 'NONE',  ( 13.09808825521931297, 34.66051412330310200, -136.0552959530295993 ) ) ;
#16561 = CARTESIAN_POINT ( 'NONE',  ( -23.53713177915716059, 38.91803379064137403, -139.7038563397429698 ) ) ;
#16562 = CARTESIAN_POINT ( 'NONE',  ( 16.65421564080000039, -18.61497348660000029, -146.5552959529999839 ) ) ;
#16563 = CYLINDRICAL_SURFACE ( 'NONE', #1243, 3.000000000000002665 ) ;
#16564 = DIRECTION ( 'NONE',  ( 0.000000000000000000, 1.000000000000000000, 0.000000000000000000 ) ) ;
#16565 = PLANE ( 'NONE',  #21444 ) ;
#16566 = ORIENTED_EDGE ( 'NONE', *, *, #10708, .F. ) ;
#16567 = LINE ( 'NONE', #278, #17474 ) ;
#16568 = VECTOR ( 'NONE', #7258, 1000.000000000000000 ) ;
#16569 = AXIS2_PLACEMENT_3D ( 'NONE', #20392, #9890, #20862 ) ;
#16570 = ORIENTED_EDGE ( 'NONE', *, *, #21864, .F. ) ;
#16571 = CARTESIAN_POINT ( 'NONE',  ( -2.499999999929999994, 40.00000000000000000, -138.0552959530000123 ) ) ;
#16572 = EDGE_CURVE ( 'NONE', #23456, #2031, #14628, .T. ) ;
#16573 = CARTESIAN_POINT ( 'NONE',  ( 31.96891336220000213, 40.94938100119999547, -149.5552959529999839 ) ) ;
#16574 = CARTESIAN_POINT ( 'NONE',  ( 25.15155135439999867, -26.08415009650000016, -147.0552959529999839 ) ) ;
#16575 = EDGE_CURVE ( 'NONE', #15711, #19530, #10916, .T. ) ;
#16576 = CARTESIAN_POINT ( 'NONE',  ( 9.683200060759999062, -20.50000000000000000, -150.0552959529999839 ) ) ;
#16577 = CARTESIAN_POINT ( 'NONE',  ( -13.27765529700754499, 34.26824771871878283, -140.3891660076678249 ) ) ;
#16578 = DIRECTION ( 'NONE',  ( 0.7633862853691524286, -0.6459422414661292189, 2.187574565940437122E-17 ) ) ;
#16579 = CARTESIAN_POINT ( 'NONE',  ( 3.611688725869999975E-11, 51.50000000000000000, -136.0552959530000123 ) ) ;
#16580 = CARTESIAN_POINT ( 'NONE',  ( -25.86630785129999666, -50.50000000000000000, -137.0552959530000123 ) ) ;
#16581 = DIRECTION ( 'NONE',  ( 0.000000000000000000, -1.000000000000000000, 0.000000000000000000 ) ) ;
#16582 = FACE_OUTER_BOUND ( 'NONE', #20274, .T. ) ;
#16583 = EDGE_LOOP ( 'NONE', ( #5997, #15377, #20204, #23037 ) ) ;
#16584 = AXIS2_PLACEMENT_3D ( 'NONE', #17901, #283, #7414 ) ;
#16585 = PRODUCT_DEFINITION_CONTEXT ( 'detailed design', #8252, 'design' ) ;
#16586 = ORIENTED_EDGE ( 'NONE', *, *, #23054, .T. ) ;
#16587 = ORIENTED_EDGE ( 'NONE', *, *, #19673, .T. ) ;
#16588 = CARTESIAN_POINT ( 'NONE',  ( -12.37691123100000112, 36.07411227369999551, -148.4862478850000116 ) ) ;
#16589 = LINE ( 'NONE', #18384, #22096 ) ;
#16590 = DIRECTION ( 'NONE',  ( 0.000000000000000000, 0.000000000000000000, 1.000000000000000000 ) ) ;
#16591 = EDGE_LOOP ( 'NONE', ( #17501, #9718, #8457, #17592 ) ) ;
#16592 = CARTESIAN_POINT ( 'NONE',  ( 24.33948587669652497, 34.09808825513344743, -136.0552959530549515 ) ) ;
#16593 = LINE ( 'NONE', #7779, #398 ) ;
#16594 = CYLINDRICAL_SURFACE ( 'NONE', #10553, 1.500000000000003331 ) ;
#16595 = ORIENTED_EDGE ( 'NONE', *, *, #620, .F. ) ;
#16596 = CARTESIAN_POINT ( 'NONE',  ( -20.49738647338961783, 39.04222973627229010, -141.2738626595669871 ) ) ;
#16597 = VECTOR ( 'NONE', #19660, 999.9999999999998863 ) ;
#16598 = EDGE_CURVE ( 'NONE', #15273, #7002, #10796, .T. ) ;
#16599 = FACE_OUTER_BOUND ( 'NONE', #20713, .T. ) ;
#16600 = AXIS2_PLACEMENT_3D ( 'NONE', #14971, #18320, #7367 ) ;
#16601 = ADVANCED_FACE ( 'NONE', ( #3804 ), #10560, .F. ) ;
#16602 = DIRECTION ( 'NONE',  ( 0.000000000000000000, 1.000000000000000000, 0.000000000000000000 ) ) ;
#16603 = DIRECTION ( 'NONE',  ( 0.000000000000000000, 0.000000000000000000, -1.000000000000000000 ) ) ;
#16604 = ORIENTED_EDGE ( 'NONE', *, *, #16732, .T. ) ;
#16605 = DIRECTION ( 'NONE',  ( 0.000000000000000000, 1.000000000000000000, 0.000000000000000000 ) ) ;
#16606 = VERTEX_POINT ( 'NONE', #23318 ) ;
#16607 =( LENGTH_UNIT ( ) NAMED_UNIT ( * ) SI_UNIT ( .MILLI., .METRE. ) );
#16609 = EDGE_LOOP ( 'NONE', ( #1630, #1866 ) ) ;
#16608 = AXIS2_PLACEMENT_3D ( 'NONE', #9392, #11296, #20141 ) ;
#16610 = CARTESIAN_POINT ( 'NONE',  ( -25.88719801257649422, 40.74404324587289494, -141.9468274994828221 ) ) ;
#16611 = VERTEX_POINT ( 'NONE', #7010 ) ;
#16612 = CARTESIAN_POINT ( 'NONE',  ( 5.219138307789999764, -2.183626157169999971, -139.5552959529999839 ) ) ;
#16613 = VECTOR ( 'NONE', #16469, 1000.000000000000000 ) ;
#16614 = ORIENTED_EDGE ( 'NONE', *, *, #7640, .T. ) ;
#16615 = CARTESIAN_POINT ( 'NONE',  ( -18.00000000000000000, -43.00000000000000000, -150.0552959529999839 ) ) ;
#16616 = ORIENTED_EDGE ( 'NONE', *, *, #12285, .F. ) ;
#16617 = SHAPE_DEFINITION_REPRESENTATION ( #9976, #17559 ) ;
#16618 = ADVANCED_FACE ( 'NONE', ( #12472 ), #12683, .F. ) ;
#16619 = ORIENTED_EDGE ( 'NONE', *, *, #14694, .T. ) ;
#16620 = CARTESIAN_POINT ( 'NONE',  ( 24.35183050010000017, -28.38413933620000051, -145.5552959529999839 ) ) ;
#16621 = CARTESIAN_POINT ( 'NONE',  ( 13.61765588494693802, 22.91567315752959644, -150.0552959529999555 ) ) ;
#16622 = CARTESIAN_POINT ( 'NONE',  ( -9.334216945200001447, -17.19633444960000190, -145.5552959529999839 ) ) ;
#16623 = CARTESIAN_POINT ( 'NONE',  ( -7.036544835898043360, 36.13414510776094346, -148.5487805666791132 ) ) ;
#16624 = CARTESIAN_POINT ( 'NONE',  ( -8.238646733050000392, 41.24792906369999912, -143.6196368420000056 ) ) ;
#16625 = ORIENTED_EDGE ( 'NONE', *, *, #7751, .F. ) ;
#16626 = DIRECTION ( 'NONE',  ( 2.257144641404620116E-12, 2.777754792983395132E-24, 1.000000000000000000 ) ) ;
#16627 = EDGE_CURVE ( 'NONE', #10172, #19035, #19579, .T. ) ;
#16628 = B_SPLINE_CURVE_WITH_KNOTS ( 'NONE', 3,
 ( #16615, #14955, #18761, #212, #4015, #14844, #450, #2119, #566, #9693, #2472, #22103, #11243, #15069, #9341, #16968, #6022, #22330 ),
 .UNSPECIFIED., .F., .F.,
 ( 4, 2, 2, 2, 2, 2, 2, 2, 4 ),
 ( 0.000000000000000000, 0.1250000000000002776, 0.2500000000000005551, 0.3750000000000008327, 0.5000000000000011102, 0.6250000000000007772, 0.7500000000000005551, 0.8750000000000002220, 1.000000000000000000 ),
 .UNSPECIFIED. ) ;
#16629 = VECTOR ( 'NONE', #415, 1000.000000000000000 ) ;
#16630 = DIRECTION ( 'NONE',  ( 1.526468026909999897E-13, 8.159623473500000156E-13, 1.000000000000000000 ) ) ;
#16631 =( GEOMETRIC_REPRESENTATION_CONTEXT ( 3 ) GLOBAL_UNCERTAINTY_ASSIGNED_CONTEXT ( ( #6604 ) ) GLOBAL_UNIT_ASSIGNED_CONTEXT ( ( #13530, #21165, #1187 ) ) REPRESENTATION_CONTEXT ( 'NONE', 'WORKASPACE' ) );
#16632 = ORIENTED_EDGE ( 'NONE', *, *, #10056, .T. ) ;
#16633 = CARTESIAN_POINT ( 'NONE',  ( 8.100000000049998761, 37.00000000000000000, -148.7552959530000010 ) ) ;
#16634 = CARTESIAN_POINT ( 'NONE',  ( -11.96343978471735880, 39.40444247627922181, -140.7635797601743093 ) ) ;
#16635 = EDGE_CURVE ( 'NONE', #20206, #7723, #11575, .T. ) ;
#16636 = CARTESIAN_POINT ( 'NONE',  ( -17.31853222291778138, 41.66660742467398393, -143.5159414623645091 ) ) ;
#16637 = CARTESIAN_POINT ( 'NONE',  ( 1.000000000140000012, 41.50000000000000000, -146.5552959529999839 ) ) ;
#16638 = ORIENTED_EDGE ( 'NONE', *, *, #16058, .T. ) ;
#16639 = DIRECTION ( 'NONE',  ( -1.000000000000000000, 0.000000000000000000, 1.701177084980000217E-20 ) ) ;
#16640 = LINE ( 'NONE', #7937, #9328 ) ;
#16641 = SHAPE_REPRESENTATION ( 'Faceplate Support', ( #5025 ), #3536 ) ;
#16642 = ORIENTED_EDGE ( 'NONE', *, *, #12600, .F. ) ;
#16643 = CARTESIAN_POINT ( 'NONE',  ( 6.750000000000000000, -47.00000000000000000, -151.0552959529999839 ) ) ;
#16644 = CARTESIAN_POINT ( 'NONE',  ( 6.000000000010000001, -3.500000000000000000, -137.0552959530000123 ) ) ;
#16645 = DIRECTION ( 'NONE',  ( 0.000000000000000000, 0.000000000000000000, -1.000000000000000000 ) ) ;
#16646 = CARTESIAN_POINT ( 'NONE',  ( -19.79317654011716243, 38.64314174742496277, -140.5356700202810032 ) ) ;
#16647 = ORIENTED_EDGE ( 'NONE', *, *, #3565, .F. ) ;
#16648 =( NAMED_UNIT ( * ) PLANE_ANGLE_UNIT ( ) SI_UNIT ( $, .RADIAN. ) );
#16649 = VECTOR ( 'NONE', #18222, 1000.000000000000000 ) ;
#16650 = ADVANCED_FACE ( 'NONE', ( #3271 ), #21132, .T. ) ;
#16651 = FACE_OUTER_BOUND ( 'NONE', #19505, .T. ) ;
#16652 = CARTESIAN_POINT ( 'NONE',  ( -3.499999999929999994, 40.00000000000000000, -138.0552959530000123 ) ) ;
#16653 = EDGE_CURVE ( 'NONE', #14749, #11085, #4943, .T. ) ;
#16654 = VECTOR ( 'NONE', #15061, 1000.000000000000000 ) ;
#16655 = FACE_OUTER_BOUND ( 'NONE', #1536, .T. ) ;
#16656 = LINE ( 'NONE', #16892, #15182 ) ;
#16657 = EDGE_CURVE ( 'NONE', #10871, #6792, #14103, .T. ) ;
#16658 = EDGE_LOOP ( 'NONE', ( #1232, #1491, #13064, #17178 ) ) ;
#16659 = DIRECTION ( 'NONE',  ( -2.257252162960000001E-12, 0.000000000000000000, -1.000000000000000000 ) ) ;
#16660 = ADVANCED_FACE ( 'NONE', ( #12066 ), #6600, .F. ) ;
#16661 = CARTESIAN_POINT ( 'NONE',  ( -38.72222222220000276, 27.75000000000000000, -140.5552959529999839 ) ) ;
#16662 = ORIENTED_EDGE ( 'NONE', *, *, #17386, .F. ) ;
#16663 = ORIENTED_EDGE ( 'NONE', *, *, #14639, .F. ) ;
#16664 = DIRECTION ( 'NONE',  ( -2.257144641399999941E-12, 0.000000000000000000, -1.000000000000000000 ) ) ;
#16665 = CIRCLE ( 'NONE', #6402, 1.499999999999999556 ) ;
#16666 = CARTESIAN_POINT ( 'NONE',  ( -29.86462848807619963, 41.46897301219815546, -145.0541174283790156 ) ) ;
#16667 = CIRCLE ( 'NONE', #5658, 2.999999999999999112 ) ;
#16668 = CARTESIAN_POINT ( 'NONE',  ( -22.52780672249999938, 37.05898997719999954, -140.0074087190000114 ) ) ;
#16669 = CARTESIAN_POINT ( 'NONE',  ( 7.609232054053188143, 35.79289365172241588, -141.8657226768378052 ) ) ;
#16670 = ORIENTED_EDGE ( 'NONE', *, *, #6442, .F. ) ;
#16671 = DIRECTION ( 'NONE',  ( 2.256861364460000137E-12, 0.000000000000000000, 1.000000000000000000 ) ) ;
#16672 = CARTESIAN_POINT ( 'NONE',  ( -20.28536656038061636, 36.96856293253166115, -139.5160734783576970 ) ) ;
#16673 = VECTOR ( 'NONE', #5205, 1000.000000000000000 ) ;
#16674 = DIRECTION ( 'NONE',  ( 0.000000000000000000, -1.000000000000000000, 0.000000000000000000 ) ) ;
#16675 = CARTESIAN_POINT ( 'NONE',  ( 6.500000000000000000, 20.50000000000000000, -150.0552959529999839 ) ) ;
#16676 = VECTOR ( 'NONE', #14884, 1000.000000000000000 ) ;
#16677 = CARTESIAN_POINT ( 'NONE',  ( -23.91265852341890508, 39.71016181377052590, -147.9043966267969665 ) ) ;
#16678 = EDGE_CURVE ( 'NONE', #7477, #16880, #12888, .T. ) ;
#16679 = CARTESIAN_POINT ( 'NONE',  ( 10.42296856120758619, -19.52552649182162270, -148.5552959529999839 ) ) ;
#16680 = EDGE_CURVE ( 'NONE', #15926, #11000, #4373, .T. ) ;
#16681 = FACE_OUTER_BOUND ( 'NONE', #15421, .T. ) ;
#16682 = CARTESIAN_POINT ( 'NONE',  ( 27.18320006080000084, 3.500000000000000000, -149.3052959529999839 ) ) ;
#16683 = CARTESIAN_POINT ( 'NONE',  ( -6.370493725010000219, -17.65251768590000125, -144.5552959529999839 ) ) ;
#16684 = AXIS2_PLACEMENT_3D ( 'NONE', #15493, #9887, #20858 ) ;
#16685 = ORIENTED_EDGE ( 'NONE', *, *, #6911, .F. ) ;
#16686 = CARTESIAN_POINT ( 'NONE',  ( -6.133959734627684846, 40.45360061668009877, -141.9452128759455434 ) ) ;
#16687 = AXIS2_PLACEMENT_3D ( 'NONE', #10259, #22532, #19433 ) ;
#16688 = ORIENTED_EDGE ( 'NONE', *, *, #2257, .T. ) ;
#16689 = DIRECTION ( 'NONE',  ( 1.000000000000000000, 0.000000000000000000, 0.000000000000000000 ) ) ;
#16690 = CIRCLE ( 'NONE', #9063, 2.000000000000000000 ) ;
#16691 = CARTESIAN_POINT ( 'NONE',  ( -22.52374396461171102, 33.50559259353841668, -144.4021133944701774 ) ) ;
#16692 = PLANE ( 'NONE',  #13624 ) ;
#16693 = VERTEX_POINT ( 'NONE', #18027 ) ;
#16694 = CARTESIAN_POINT ( 'NONE',  ( -12.53599637006591827, 32.89425847576748652, -144.5669343789962511 ) ) ;
#16695 = CARTESIAN_POINT ( 'NONE',  ( -5.316799939240000938, 3.500000000000000000, -150.0552959529999839 ) ) ;
#16696 = CARTESIAN_POINT ( 'NONE',  ( 15.10234832539273420, 33.50000000000000000, -150.0552959530000123 ) ) ;
#16697 = DIRECTION ( 'NONE',  ( -1.000000000000000000, 0.000000000000000000, 2.257144641399999941E-12 ) ) ;
#16698 = DIRECTION ( 'NONE',  ( 0.000000000000000000, -1.000000000000000000, 0.000000000000000000 ) ) ;
#16699 = DIRECTION ( 'NONE',  ( 1.000000000000000000, 0.000000000000000000, -2.257453483404484831E-12 ) ) ;
#16700 = AXIS2_PLACEMENT_3D ( 'NONE', #4649, #11891, #11530 ) ;
#16701 = ORIENTED_EDGE ( 'NONE', *, *, #20108, .T. ) ;
#16702 = VECTOR ( 'NONE', #7459, 1000.000000000000000 ) ;
#16703 = CARTESIAN_POINT ( 'NONE',  ( -35.47299999999999898, 14.00000000000000000, -144.0552959529999839 ) ) ;
#16704 = ORIENTED_EDGE ( 'NONE', *, *, #20447, .F. ) ;
#16705 = ADVANCED_FACE ( 'NONE', ( #21487 ), #19689, .F. ) ;
#16706 = VECTOR ( 'NONE', #19637, 1000.000000000000114 ) ;
#16707 = CIRCLE ( 'NONE', #10994, 0.7500000000000006661 ) ;
#16708 = VERTEX_POINT ( 'NONE', #1627 ) ;
#16709 = CARTESIAN_POINT ( 'NONE',  ( -13.09712973210239895, 32.88797929499759931, -146.6032212821853022 ) ) ;
#16710 = DIRECTION ( 'NONE',  ( 0.000000000000000000, -1.000000000000000000, 0.000000000000000000 ) ) ;
#16711 = CARTESIAN_POINT ( 'NONE',  ( 22.40884248670000289, -21.39641658300000060, -143.5552959529999839 ) ) ;
#16712 = ORIENTED_EDGE ( 'NONE', *, *, #3474, .F. ) ;
#16713 = DIRECTION ( 'NONE',  ( 1.527666881879999979E-13, 8.153477892850000134E-13, 1.000000000000000000 ) ) ;
#16714 = LINE ( 'NONE', #427, #15589 ) ;
#16715 = CARTESIAN_POINT ( 'NONE',  ( -9.334216945200001447, -17.19633444960000190, -145.5552959529999839 ) ) ;
#16716 = VERTEX_POINT ( 'NONE', #5287 ) ;
#16717 = CARTESIAN_POINT ( 'NONE',  ( -20.74418227170635731, 39.28578094490452344, -147.3492911869098236 ) ) ;
#16718 = B_SPLINE_CURVE_WITH_KNOTS ( 'NONE', 3,
 ( #17866, #14412, #7146, #19890, #5486, #142, #12618, #3823, #7384, #1935 ),
 .UNSPECIFIED., .F., .F.,
 ( 4, 2, 2, 2, 4 ),
 ( 0.000000000000000000, 0.2500000000000000000, 0.5000000000000000000, 0.7500000000000000000, 1.000000000000000000 ),
 .UNSPECIFIED. ) ;
#16719 = CARTESIAN_POINT ( 'NONE',  ( 9.633444787484091165, 37.98285379039364074, -141.7565619020742531 ) ) ;
#16720 = VECTOR ( 'NONE', #17063, 999.9999999999998863 ) ;
#16721 = VECTOR ( 'NONE', #20622, 1000.000000000000000 ) ;
#16722 = CARTESIAN_POINT ( 'NONE',  ( 6.500000000149999124, 20.50000000000000000, -143.5552959529999839 ) ) ;
#16723 = AXIS2_PLACEMENT_3D ( 'NONE', #5452, #16400, #9117 ) ;
#16724 = CARTESIAN_POINT ( 'NONE',  ( -31.50000000000000000, -50.00000000000000000, -143.3052959529999839 ) ) ;
#16725 = VERTEX_POINT ( 'NONE', #12537 ) ;
#16726 = LINE ( 'NONE', #20656, #13720 ) ;
#16727 = ORIENTED_EDGE ( 'NONE', *, *, #16898, .F. ) ;
#16728 = CARTESIAN_POINT ( 'NONE',  ( 7.759759976955875160, -48.74600213680044192, -150.0552959529999839 ) ) ;
#16729 = ORIENTED_EDGE ( 'NONE', *, *, #13766, .T. ) ;
#16730 = CARTESIAN_POINT ( 'NONE',  ( -26.57320955767643511, 39.25615809526139799, -147.2502486967401580 ) ) ;
#16731 = ORIENTED_EDGE ( 'NONE', *, *, #1498, .F. ) ;
#16732 = EDGE_CURVE ( 'NONE', #7451, #7250, #19466, .T. ) ;
#16733 = CARTESIAN_POINT ( 'NONE',  ( -22.23138069772303638, 34.62558912635464026, -140.6296127985235955 ) ) ;
#16734 = ORIENTED_EDGE ( 'NONE', *, *, #19490, .T. ) ;
#16735 = CARTESIAN_POINT ( 'NONE',  ( -30.02199999990000023, 40.03108891319999429, -145.8052959529999839 ) ) ;
#16736 = EDGE_CURVE ( 'NONE', #15302, #7477, #1738, .T. ) ;
#16737 = EDGE_LOOP ( 'NONE', ( #8306, #5194, #6367, #23228 ) ) ;
#16738 = APPLICATION_PROTOCOL_DEFINITION ( 'draft international standard', 'automotive_design', 1998, #20893 ) ;
#16739 = VECTOR ( 'NONE', #14878, 1000.000000000000227 ) ;
#16740 = ORIENTED_EDGE ( 'NONE', *, *, #8375, .F. ) ;
#16741 = CARTESIAN_POINT ( 'NONE',  ( -27.22834295012582828, 41.68433299786980939, -144.4761705782878209 ) ) ;
#16742 = CARTESIAN_POINT ( 'NONE',  ( -4.500000000000000000, 34.00000000000000000, -151.0552959529999839 ) ) ;
#16743 = CYLINDRICAL_SURFACE ( 'NONE', #5028, 24.99999999999999645 ) ;
#16744 = LINE ( 'NONE', #13168, #10947 ) ;
#16745 = CARTESIAN_POINT ( 'NONE',  ( -6.071644824238406457, 36.06915794949389920, -148.2800132152668766 ) ) ;
#16746 = CARTESIAN_POINT ( 'NONE',  ( -8.712023184163379952, 38.57885015659952188, -140.3122811010784119 ) ) ;
#16747 = EDGE_LOOP ( 'NONE', ( #7864, #21731, #10646, #17882, #1197 ) ) ;
#16748 = CARTESIAN_POINT ( 'NONE',  ( -1.500000000000000000, 44.50000000000000000, -150.0552959529999839 ) ) ;
#16749 = ADVANCED_FACE ( 'NONE', ( #22918 ), #8498, .F. ) ;
#16750 = DIRECTION ( 'NONE',  ( 0.000000000000000000, 0.000000000000000000, 1.000000000000000000 ) ) ;
#16751 = DIRECTION ( 'NONE',  ( 2.257157423930000049E-12, 0.000000000000000000, 1.000000000000000000 ) ) ;
#16752 = VECTOR ( 'NONE', #1357, 1000.000000000000000 ) ;
#16753 = ORIENTED_EDGE ( 'NONE', *, *, #22750, .T. ) ;
#16754 = VECTOR ( 'NONE', #12031, 1000.000000000000000 ) ;
#16755 = DIRECTION ( 'NONE',  ( 2.507554887169999917E-12, 0.000000000000000000, -1.000000000000000000 ) ) ;
#16756 = CARTESIAN_POINT ( 'NONE',  ( -12.35807366786784911, 40.97448640521876229, -143.6870081750666657 ) ) ;
#16757 = DIRECTION ( 'NONE',  ( -1.000000000000000000, 5.094701932209999624E-24, 2.257144641399999941E-12 ) ) ;
#16758 = CARTESIAN_POINT ( 'NONE',  ( 20.50000000000000000, 25.50000000000000000, -151.0552959529999839 ) ) ;
#16759 = EDGE_LOOP ( 'NONE', ( #17466, #8282, #3642, #3146 ) ) ;
#16760 = DIRECTION ( 'NONE',  ( 2.507554887169999917E-12, 0.000000000000000000, -1.000000000000000000 ) ) ;
#16761 = CARTESIAN_POINT ( 'NONE',  ( -30.02199999990000023, 40.03108891319999429, -145.8052959529999839 ) ) ;
#16762 = VERTEX_POINT ( 'NONE', #12189 ) ;
#16763 = CARTESIAN_POINT ( 'NONE',  ( -31.75000000000000000, -36.00000000000000000, -151.0552959529999839 ) ) ;
#16764 = CARTESIAN_POINT ( 'NONE',  ( -29.13601448249999848, 36.98639052360000079, -140.5419328609999923 ) ) ;
#16765 = ORIENTED_EDGE ( 'NONE', *, *, #17841, .F. ) ;
#16766 = FACE_OUTER_BOUND ( 'NONE', #5875, .T. ) ;
#16767 = CARTESIAN_POINT ( 'NONE',  ( -21.70878449369999785, 39.52018264390000013, -147.4849246469999855 ) ) ;
#16768 = ORIENTED_EDGE ( 'NONE', *, *, #7751, .T. ) ;
#16769 = SURFACE_STYLE_USAGE ( .BOTH. , #6061 ) ;
#16770 = FACE_OUTER_BOUND ( 'NONE', #9933, .T. ) ;
#16771 = DIRECTION ( 'NONE',  ( 0.000000000000000000, 2.256988247090000272E-12, 1.000000000000000000 ) ) ;
#16772 = ORIENTED_EDGE ( 'NONE', *, *, #14197, .T. ) ;
#16773 = DIRECTION ( 'NONE',  ( 1.000000000000000000, 0.000000000000000000, 0.000000000000000000 ) ) ;
#16774 = LINE ( 'NONE', #16542, #9173 ) ;
#16775 = VECTOR ( 'NONE', #20718, 1000.000000000000000 ) ;
#16776 = DIRECTION ( 'NONE',  ( 1.000000000000000000, 0.000000000000000000, 2.516505522483685870E-12 ) ) ;
#16777 = CLOSED_SHELL ( 'NONE', ( #15720, #12563, #10241, #21755, #5662, #20409, #14933, #2781, #1385, #9503, #20913, #17817, #8480, #20071, #6608, #22739, #18454, #11410, #3508, #12887, #9600, #2998, #19023, #16452, #4818, #22774, #4310, #13570, #6559, #22533, #13321, #22026, #5279, #13005, #4628, #5207, #11455, #799, #9676, #17194, #7057, #17939, #9199, #10813, #8462, #23273, #21153, #7845, #4171, #13084, #21935, #1992, #21741, #5464, #15553, #6711, #512, #9093, #14488, #7899, #1851, #475, #1817, #10890, #13582, #5667, #14349, #11253, #14403, #16377, #12781, #12410, #4219, #19154, #9669, #11826, #2354, #3611, #12561, #3267, #4002, #821, #20857, #8191, #21749, #19690, #5322, #440, #9409, #22494, #5539, #10893, #332, #2823, #13887, #2091, #17247, #5468, #16650, #8080, #19065, #1739, #22185, #15846, #12482, #16705, #6038, #5879, #17967, #17252, #2973, #22846, #6794, #12687, #21611, #12584, #6528, #22273, #3738, #20888, #17522, #13769, #222, #19515, #8685, #14782, #17810, #4572, #20376, #16867, #14895, #13759, #2806, #11639, #7968, #4308, #19517, #13178, #9655, #5323, #13080, #7199, #14159 ) ) ;
#16778 = VECTOR ( 'NONE', #22869, 1000.000000000000000 ) ;
#16779 = ORIENTED_EDGE ( 'NONE', *, *, #20615, .T. ) ;
#16780 = CARTESIAN_POINT ( 'NONE',  ( 11.68320006079999906, -20.50000000000000000, -148.5552959529999839 ) ) ;
#16781 = EDGE_CURVE ( 'NONE', #22145, #941, #18425, .T. ) ;
#16782 = CARTESIAN_POINT ( 'NONE',  ( 6.000000000140000012, 32.99305018889999275, -147.5552959529999839 ) ) ;
#16783 = ORIENTED_EDGE ( 'NONE', *, *, #21236, .F. ) ;
#16784 = APPLICATION_CONTEXT ( 'automotive_design' ) ;
#16785 = ORIENTED_EDGE ( 'NONE', *, *, #6740, .T. ) ;
#16786 = LINE ( 'NONE', #2058, #18860 ) ;
#16787 = EDGE_CURVE ( 'NONE', #3797, #9003, #15878, .T. ) ;
#16788 = LINE ( 'NONE', #502, #2857 ) ;
#16789 = EDGE_CURVE ( 'NONE', #5687, #1422, #9421, .T. ) ;
#16790 = LINE ( 'NONE', #18235, #11654 ) ;
#16791 = CARTESIAN_POINT ( 'NONE',  ( 7.883839590577690792, 35.63231902296612930, -141.9625758180283128 ) ) ;
#16792 = VERTEX_POINT ( 'NONE', #19929 ) ;
#16793 = VECTOR ( 'NONE', #18329, 1000.000000000000114 ) ;
#16794 = VECTOR ( 'NONE', #8367, 1000.000000000000000 ) ;
#16795 = CARTESIAN_POINT ( 'NONE',  ( -7.149448239889999890, -25.45628515800000002, -145.5552959529999839 ) ) ;
#16796 = VECTOR ( 'NONE', #8332, 1000.000000000000000 ) ;
#16797 = EDGE_CURVE ( 'NONE', #6475, #20332, #8962, .T. ) ;
#16798 = CARTESIAN_POINT ( 'NONE',  ( 14.79224200838147318, -1.499999999999999778, -141.9623572382618306 ) ) ;
#16799 = CARTESIAN_POINT ( 'NONE',  ( 15.10234832544105643, 33.50000000000002132, -136.0552959530340331 ) ) ;
#16800 = EDGE_CURVE ( 'NONE', #22948, #8011, #20335, .T. ) ;
#16801 = LINE ( 'NONE', #7743, #15529 ) ;
#16802 = CARTESIAN_POINT ( 'NONE',  ( -32.50000000000000000, 76.00000000000000000, -144.0552959529999839 ) ) ;
#16803 = PLANE ( 'NONE',  #18317 ) ;
#16804 = DIRECTION ( 'NONE',  ( 1.000000000000000000, 0.000000000000000000, -1.498801083243961330E-13 ) ) ;
#16805 = CARTESIAN_POINT ( 'NONE',  ( -29.18315392600000280, -51.50000000000000000, -136.0552959530000123 ) ) ;
#16806 = ORIENTED_EDGE ( 'NONE', *, *, #3389, .F. ) ;
#16807 = CARTESIAN_POINT ( 'NONE',  ( -6.909346445838660422, 37.92300339050624558, -148.1333867873858026 ) ) ;
#16808 = LINE ( 'NONE', #7637, #18348 ) ;
#16809 = EDGE_CURVE ( 'NONE', #8740, #416, #3629, .T. ) ;
#16810 = ORIENTED_EDGE ( 'NONE', *, *, #11423, .T. ) ;
#16811 = EDGE_CURVE ( 'NONE', #8391, #19898, #9073, .T. ) ;
#16812 = AXIS2_PLACEMENT_3D ( 'NONE', #15810, #20817, #11877 ) ;
#16813 = CARTESIAN_POINT ( 'NONE',  ( -21.76391789540379662, 33.32496974993136973, -144.3326792069850626 ) ) ;
#16814 = DIRECTION ( 'NONE',  ( 4.510774274160000731E-12, -1.321907670990000086E-13, 1.000000000000000000 ) ) ;
#16815 = ORIENTED_EDGE ( 'NONE', *, *, #13877, .T. ) ;
#16816 = CARTESIAN_POINT ( 'NONE',  ( -12.37691123100000112, 36.07411227369999551, -148.4862478850000116 ) ) ;
#16817 = ADVANCED_FACE ( 'NONE', ( #12893 ), #20174, .F. ) ;
#16818 = DIRECTION ( 'NONE',  ( 0.000000000000000000, -1.000000000000000000, 3.568879590630000244E-13 ) ) ;
#16819 = EDGE_CURVE ( 'NONE', #6070, #19806, #11957, .T. ) ;
#16820 = CARTESIAN_POINT ( 'NONE',  ( 12.57650987475213533, 37.28094649259004711, -150.0552959529999839 ) ) ;
#16821 = ITEM_DEFINED_TRANSFORMATION ( 'NONE', 'NONE', #3179,  #5025 ) ;
#16822 = CARTESIAN_POINT ( 'NONE',  ( 4.499999999879999102, -3.000000000000000000, -135.4552959529999896 ) ) ;
#16823 = DIRECTION ( 'NONE',  ( 0.000000000000000000, 1.000000000000000000, 0.000000000000000000 ) ) ;
#16824 = EDGE_CURVE ( 'NONE', #15695, #8634, #20396, .T. ) ;
#16825 = LINE ( 'NONE', #180, #10161 ) ;
#16826 = ORIENTED_EDGE ( 'NONE', *, *, #16953, .F. ) ;
#16827 = COLOUR_RGB ( '', 0.08235294, 0.09019608, 0.10196078) ;
#16828 = AXIS2_PLACEMENT_3D ( 'NONE', #19651, #3232, #4900 ) ;
#16829 = CARTESIAN_POINT ( 'NONE',  ( -28.15861914003539468, 32.75082038491409975, -146.4619352604428286 ) ) ;
#16830 = VERTEX_POINT ( 'NONE', #10861 ) ;
#16831 = PRESENTATION_STYLE_ASSIGNMENT (( #8119 ) ) ;
#16832 = EDGE_LOOP ( 'NONE', ( #4209, #18332, #3619, #5535 ) ) ;
#16833 = CARTESIAN_POINT ( 'NONE',  ( -18.00000000000000000, -43.00000000000000000, -145.5552959529999839 ) ) ;
#16834 = CARTESIAN_POINT ( 'NONE',  ( -9.934356875269999776, -23.16624500709999879, -146.0552959529999839 ) ) ;
#16835 = DIRECTION ( 'NONE',  ( 0.000000000000000000, -1.000000000000000000, 0.000000000000000000 ) ) ;
#16836 = EDGE_LOOP ( 'NONE', ( #4589, #7295, #2681, #11812, #9712, #10588, #21513 ) ) ;
#16837 = DIRECTION ( 'NONE',  ( 2.259525899719999991E-12, 0.000000000000000000, 1.000000000000000000 ) ) ;
#16838 = LINE ( 'NONE', #6120, #16720 ) ;
#16839 = ORIENTED_EDGE ( 'NONE', *, *, #22546, .T. ) ;
#16840 = CARTESIAN_POINT ( 'NONE',  ( 13.05339791269693528, 16.72285764721824819, -136.0552959530147348 ) ) ;
#16841 = CARTESIAN_POINT ( 'NONE',  ( 9.390767940384391110, 38.20710635247810671, -141.8657226791105188 ) ) ;
#16842 = AXIS2_PLACEMENT_3D ( 'NONE', #8999, #5454, #7238 ) ;
#16843 = EDGE_CURVE ( 'NONE', #9722, #6969, #19201, .T. ) ;
#16844 = CARTESIAN_POINT ( 'NONE',  ( 32.50000000000000000, -40.50000000000000000, -137.0552959530000123 ) ) ;
#16845 = ADVANCED_FACE ( 'NONE', ( #20048 ), #21727, .T. ) ;
#16846 = CARTESIAN_POINT ( 'NONE',  ( -27.60583033836061517, 37.01000650955438687, -148.6900182103051691 ) ) ;
#16847 = VERTEX_POINT ( 'NONE', #11325 ) ;
#16848 = CARTESIAN_POINT ( 'NONE',  ( 4.999999999879999990, -4.000000000000000000, -135.0552959530000123 ) ) ;
#16849 = ORIENTED_EDGE ( 'NONE', *, *, #19791, .T. ) ;
#16850 = SURFACE_SIDE_STYLE ('',( #22095 ) ) ;
#16851 = VERTEX_POINT ( 'NONE', #16361 ) ;
#16852 = CARTESIAN_POINT ( 'NONE',  ( -26.39607007120000048, 36.95534867429999792, -140.3840478969999879 ) ) ;
#16853 = ORIENTED_EDGE ( 'NONE', *, *, #9220, .F. ) ;
#16854 = CARTESIAN_POINT ( 'NONE',  ( -22.92066848189358552, 37.01209555897772674, -139.3757315019954319 ) ) ;
#16855 = VERTEX_POINT ( 'NONE', #10984 ) ;
#16856 = PLANE ( 'NONE',  #20860 ) ;
#16857 = ORIENTED_EDGE ( 'NONE', *, *, #9632, .T. ) ;
#16858 = ORIENTED_EDGE ( 'NONE', *, *, #3963, .F. ) ;
#16859 = CARTESIAN_POINT ( 'NONE',  ( -27.26567793353847691, 36.96940380708128515, -148.4835048635911789 ) ) ;
#16860 = CARTESIAN_POINT ( 'NONE',  ( -7.816799939239999162, -1.500000000000000000, -150.0552959529999839 ) ) ;
#16861 = CARTESIAN_POINT ( 'NONE',  ( 9.824773488038593072, 27.24096059670178249, -150.0552959529999555 ) ) ;
#16862 = CARTESIAN_POINT ( 'NONE',  ( 25.31684607480000082, -45.26810052389999584, -136.0552959530000123 ) ) ;
#16863 = CARTESIAN_POINT ( 'NONE',  ( -6.263809632758733592, 36.02430696941269872, -148.6165307568110734 ) ) ;
#16864 = LINE ( 'NONE', #691, #12489 ) ;
#16865 = ORIENTED_EDGE ( 'NONE', *, *, #5021, .T. ) ;
#16866 = CARTESIAN_POINT ( 'NONE',  ( -32.50000000000000000, -18.00000000000000000, -140.0552959529999839 ) ) ;
#16867 = ADVANCED_FACE ( 'NONE', ( #5416 ), #12774, .T. ) ;
#16868 = EDGE_CURVE ( 'NONE', #22098, #12475, #1977, .T. ) ;
#16869 = FACE_OUTER_BOUND ( 'NONE', #23294, .T. ) ;
#16870 = CARTESIAN_POINT ( 'NONE',  ( 2.048233066679999936, -63.64014441970000746, -143.5552959529999839 ) ) ;
#16871 = ADVANCED_FACE ( 'NONE', ( #2088 ), #14578, .T. ) ;
#16872 = ORIENTED_EDGE ( 'NONE', *, *, #16525, .F. ) ;
#16873 = CARTESIAN_POINT ( 'NONE',  ( -12.48399912348327945, 39.13586957966980151, -147.0556079066718098 ) ) ;
#16874 = VECTOR ( 'NONE', #14788, 1000.000000000000000 ) ;
#16875 = CARTESIAN_POINT ( 'NONE',  ( -17.60582215389345251, 39.60819216315037750, -147.6714151693956580 ) ) ;
#16876 = FACE_OUTER_BOUND ( 'NONE', #4740, .T. ) ;
#16877 = VERTEX_POINT ( 'NONE', #9197 ) ;
#16878 = CARTESIAN_POINT ( 'NONE',  ( -8.271665395472865612, 36.97019838864552810, -139.4157638768302832 ) ) ;
#16879 = DIRECTION ( 'NONE',  ( 0.1824094679249879947, 0.9832226533249336375, -8.292396948119437334E-13 ) ) ;
#16880 = VERTEX_POINT ( 'NONE', #178 ) ;
#16881 = CARTESIAN_POINT ( 'NONE',  ( -22.00705883600000234, 37.05789963359999462, -148.1619053240000028 ) ) ;
#16882 = LINE ( 'NONE', #16425, #20605 ) ;
#16883 = VERTEX_POINT ( 'NONE', #11209 ) ;
#16884 = CARTESIAN_POINT ( 'NONE',  ( -5.449075813550353864, 45.02080533206300572, -150.0552959530000123 ) ) ;
#16885 = CARTESIAN_POINT ( 'NONE',  ( -20.02720694385126876, 38.00365282337508432, -139.3916297347710156 ) ) ;
#16886 = ORIENTED_EDGE ( 'NONE', *, *, #1766, .T. ) ;
#16887 = CARTESIAN_POINT ( 'NONE',  ( -28.11832915603455874, 33.48892755769719543, -144.3678690803285463 ) ) ;
#16888 = CYLINDRICAL_SURFACE ( 'NONE', #8379, 1.499999999999999556 ) ;
#16889 = VERTEX_POINT ( 'NONE', #14683 ) ;
#16890 = LINE ( 'NONE', #16652, #18966 ) ;
#16891 = CARTESIAN_POINT ( 'NONE',  ( 18.18320006080000084, -6.500000000000000000, -149.3052959529999839 ) ) ;
#16892 = CARTESIAN_POINT ( 'NONE',  ( 32.00000000000000000, 40.03620104880000241, -150.0552959529999839 ) ) ;
#16893 = EDGE_LOOP ( 'NONE', ( #21162, #5177, #20311, #22323 ) ) ;
#16894 = LINE ( 'NONE', #6763, #18580 ) ;
#16895 = CARTESIAN_POINT ( 'NONE',  ( 19.13369214859999801, 50.50000000000000000, -137.0552959530000123 ) ) ;
#16896 = VERTEX_POINT ( 'NONE', #21953 ) ;
#16897 = ADVANCED_BREP_SHAPE_REPRESENTATION ( '', ( #12179, #5025 ), #1616 ) ;
#16898 = EDGE_CURVE ( 'NONE', #22304, #12661, #292, .T. ) ;
#16899 = ORIENTED_EDGE ( 'NONE', *, *, #4295, .F. ) ;
#16900 = CARTESIAN_POINT ( 'NONE',  ( -23.29130810115783845, 35.45552060375986514, -140.6454276014299012 ) ) ;
#16901 = CARTESIAN_POINT ( 'NONE',  ( -30.50301086745307444, 40.75553727831436390, -144.8176898276264239 ) ) ;
#16902 = DIRECTION ( 'NONE',  ( 1.000000000000000000, 0.000000000000000000, -2.257453483404482811E-12 ) ) ;
#16903 = CARTESIAN_POINT ( 'NONE',  ( 7.708627906697441468, 35.72455532609014028, -141.9048323918832750 ) ) ;
#16904 = EDGE_LOOP ( 'NONE', ( #18450, #8052, #20303, #3489 ) ) ;
#16905 = CARTESIAN_POINT ( 'NONE',  ( 22.01137100460000084, -15.39610142400000115, -146.5552959529999839 ) ) ;
#16906 = CARTESIAN_POINT ( 'NONE',  ( -8.343166633029998280, 41.26425690090000131, -144.5268661329999986 ) ) ;
#16907 = CARTESIAN_POINT ( 'NONE',  ( -15.39061678755858864, -41.53835085783378389, -150.0552959529999839 ) ) ;
#16908 = CARTESIAN_POINT ( 'NONE',  ( -9.971101149720000834, 37.05360750090000721, -147.8421425029999909 ) ) ;
#16909 = CARTESIAN_POINT ( 'NONE',  ( -23.87836733110767540, 41.18897180524523804, -141.6563648539963367 ) ) ;
#16910 = EDGE_CURVE ( 'NONE', #12787, #7959, #15401, .T. ) ;
#16911 = AXIS2_PLACEMENT_3D ( 'NONE', #6195, #7735, #380 ) ;
#16912 = CARTESIAN_POINT ( 'NONE',  ( -14.93328160137761351, 36.92972691758927084, -148.3740393307602119 ) ) ;
#16913 = CARTESIAN_POINT ( 'NONE',  ( -16.11775386674015564, 33.36946837792675780, -144.2542744048583927 ) ) ;
#16914 = CARTESIAN_POINT ( 'NONE',  ( -20.34672008420000111, 36.01786665889999739, -139.8153362750000213 ) ) ;
#16915 = CARTESIAN_POINT ( 'NONE',  ( 18.18320006080000084, 0.4999999999990000776, -148.5552959529999839 ) ) ;
#16916 = CARTESIAN_POINT ( 'NONE',  ( -2.499999999839999987, 41.50000000000000000, -140.5552959529999839 ) ) ;
#16917 = EDGE_CURVE ( 'NONE', #15057, #13175, #766, .T. ) ;
#16918 = EDGE_LOOP ( 'NONE', ( #9366, #3433, #21570, #5449 ) ) ;
#16919 = CARTESIAN_POINT ( 'NONE',  ( -6.103115051414089720, 40.52053609467341744, -143.6011192969590127 ) ) ;
#16920 = CARTESIAN_POINT ( 'NONE',  ( 15.87827223000000032, -26.60524292859999917, -143.5552959529999839 ) ) ;
#16921 = ORIENTED_EDGE ( 'NONE', *, *, #19443, .T. ) ;
#16922 =( BOUNDED_SURFACE ( )  B_SPLINE_SURFACE ( 5, 5, ( 
 ( #21324, #10461, #17738, #8675, #22627, #13571 ),
 ( #20843, #4538, #19057, #9993, #20973, #2878 ),
 ( #19889, #1696, #14410, #1580, #3465, #3822 ),
 ( #1934, #2049, #10703, #14644, #21440, #16198 ),
 ( #24, #7383, #9153, #5595, #14537, #21684 ),
 ( #8803, #17985, #16314, #16080, #18098, #5368 ),
 ( #12617, #3586, #5123, #21914, #17864, #6912 ),
 ( #7268, #1809, #10815, #9028, #8915, #21800 ),
 ( #15958, #5485, #7145, #23335, #12731, #18218 ),
 ( #19645, #12845, #16435, #20003, #14176, #20123 ),
 ( #3698, #21557, #7027, #10936, #11057, #18338 ),
 ( #141, #23219, #12369, #3342, #10578, #14289 ) ),
 .UNSPECIFIED., .F., .F., .F. ) 
 B_SPLINE_SURFACE_WITH_KNOTS ( ( 6, 3, 3, 6 ),
 ( 6, 6 ),
 ( 0.000000000000000000, 4.445608688430000122, 8.917804078430000558, 13.41780914199999941 ),
 ( 1.570796326447220004, 3.141592653590000062 ),
 .UNSPECIFIED. ) 
 GEOMETRIC_REPRESENTATION_ITEM ( )  RATIONAL_B_SPLINE_SURFACE ( (
 ( 0.2500000000000000000, 0.2499999999557195041, 0.2999999999335790091, 0.3999999999114384752, 0.5999999999114390414, 1.000000000000000000),
 ( 0.2500000000000000000, 0.2499999999557195041, 0.2999999999335790091, 0.3999999999114384752, 0.5999999999114390414, 1.000000000000000000),
 ( 0.2500000000000000000, 0.2499999999557195041, 0.2999999999335790091, 0.3999999999114384752, 0.5999999999114390414, 1.000000000000000000),
 ( 0.2500000000000000000, 0.2499999999557195041, 0.2999999999335790091, 0.3999999999114384752, 0.5999999999114390414, 1.000000000000000000),
 ( 0.2500000000000000000, 0.2499999999557195041, 0.2999999999335790091, 0.3999999999114384752, 0.5999999999114390414, 1.000000000000000000),
 ( 0.2500000000000000000, 0.2499999999557195041, 0.2999999999335790091, 0.3999999999114384752, 0.5999999999114390414, 1.000000000000000000),
 ( 0.2500000000000000000, 0.2499999999557195041, 0.2999999999335790091, 0.3999999999114384752, 0.5999999999114390414, 1.000000000000000000),
 ( 0.2500000000000000000, 0.2499999999557195041, 0.2999999999335790091, 0.3999999999114384752, 0.5999999999114390414, 1.000000000000000000),
 ( 0.2500000000000000000, 0.2499999999557195041, 0.2999999999335790091, 0.3999999999114384752, 0.5999999999114390414, 1.000000000000000000),
 ( 0.2500000000000000000, 0.2499999999557195041, 0.2999999999335790091, 0.3999999999114384752, 0.5999999999114390414, 1.000000000000000000),
 ( 0.2500000000000000000, 0.2499999999557195041, 0.2999999999335790091, 0.3999999999114384752, 0.5999999999114390414, 1.000000000000000000),
 ( 0.2500000000000000000, 0.2499999999557195041, 0.2999999999335790091, 0.3999999999114384752, 0.5999999999114390414, 1.000000000000000000) ) ) 
 REPRESENTATION_ITEM ( '' )  SURFACE ( )  );
#16924 = VECTOR ( 'NONE', #13364, 1000.000000000000000 ) ;
#16923 = CARTESIAN_POINT ( 'NONE',  ( -21.53618355982399635, 33.35162261389687188, -146.0341402270590265 ) ) ;
#16925 = EDGE_CURVE ( 'NONE', #15915, #18797, #17047, .T. ) ;
#16926 = VECTOR ( 'NONE', #2691, 1000.000000000000000 ) ;
#16927 = CARTESIAN_POINT ( 'NONE',  ( -32.50000000000000000, -74.00000000000000000, -155.5552959529999839 ) ) ;
#16928 = VERTEX_POINT ( 'NONE', #20747 ) ;
#16929 = CARTESIAN_POINT ( 'NONE',  ( -12.30251875917725179, 34.86346480590818686, -147.0212501965618230 ) ) ;
#16930 = DIRECTION ( 'NONE',  ( 0.000000000000000000, 0.000000000000000000, 1.000000000000000000 ) ) ;
#16931 = LINE ( 'NONE', #7875, #3303 ) ;
#16932 = DIRECTION ( 'NONE',  ( -2.258193632089999862E-12, 0.000000000000000000, -1.000000000000000000 ) ) ;
#16933 = CARTESIAN_POINT ( 'NONE',  ( -32.50000000000000000, 1.000000000000000000, -143.3052959529999839 ) ) ;
#16934 = LINE ( 'NONE', #15032, #8650 ) ;
#16935 = EDGE_CURVE ( 'NONE', #6123, #7827, #9198, .T. ) ;
#16936 = VERTEX_POINT ( 'NONE', #22293 ) ;
#16937 = CARTESIAN_POINT ( 'NONE',  ( 12.01554901919999985, -37.47280209340000567, -145.5552959529999839 ) ) ;
#16938 = B_SPLINE_CURVE_WITH_KNOTS ( 'NONE', 3,
 ( #13830, #10242, #22745, #5128, #19653, #17278, #21212, #6447, #4901, #13706, #10119, #15614, #21093, #17512, #1235, #8460, #21920, #20250 ),
 .UNSPECIFIED., .F., .F.,
 ( 4, 2, 2, 2, 2, 2, 2, 2, 4 ),
 ( 0.000000000000000000, 0.1250000000000000000, 0.2500000000000000000, 0.3750000000000000000, 0.5000000000000000000, 0.6250000000000000000, 0.7500000000000000000, 0.8750000000000000000, 1.000000000000000000 ),
 .UNSPECIFIED. ) ;
#16939 = VERTEX_POINT ( 'NONE', #20992 ) ;
#16940 = VECTOR ( 'NONE', #8663, 1000.000000000000000 ) ;
#16941 = CARTESIAN_POINT ( 'NONE',  ( -13.92295968795637506, 34.11491018883658199, -140.3106646644930890 ) ) ;
#16942 = CARTESIAN_POINT ( 'NONE',  ( -9.347107914279998653, -17.32706600430000066, -144.5552959529999839 ) ) ;
#16943 = AXIS2_PLACEMENT_3D ( 'NONE', #20742, #4210, #9656 ) ;
#16944 = CARTESIAN_POINT ( 'NONE',  ( 10.68320006080000084, -20.50000000000000000, -150.0552959529999839 ) ) ;
#16945 = ADVANCED_FACE ( 'NONE', ( #6226 ), #13721, .T. ) ;
#16946 = EDGE_LOOP ( 'NONE', ( #15187, #5095 ) ) ;
#16947 = LINE ( 'NONE', #7547, #13682 ) ;
#16948 = DIRECTION ( 'NONE',  ( 1.000000000000000000, -5.094701932209999624E-24, 0.000000000000000000 ) ) ;
#16949 = EDGE_CURVE ( 'NONE', #11927, #15664, #11801, .T. ) ;
#16950 = ORIENTED_EDGE ( 'NONE', *, *, #9133, .T. ) ;
#16951 = CARTESIAN_POINT ( 'NONE',  ( -21.29590688489999906, 41.28591597809999314, -144.5271551099999954 ) ) ;
#16952 = EDGE_CURVE ( 'NONE', #5601, #3284, #6462, .T. ) ;
#16953 = EDGE_CURVE ( 'NONE', #4267, #21050, #17173, .T. ) ;
#16954 = CARTESIAN_POINT ( 'NONE',  ( 9.338468952632505093, 38.24377360218669963, -141.8866492539555111 ) ) ;
#16955 = CARTESIAN_POINT ( 'NONE',  ( 7.874234281797447110, 35.63651660423768419, -146.1507818849889873 ) ) ;
#16956 = LINE ( 'NONE', #15176, #6294 ) ;
#16957 = AXIS2_PLACEMENT_3D ( 'NONE', #9514, #7617, #18349 ) ;
#16958 = CARTESIAN_POINT ( 'NONE',  ( 6.499999999879999102, -3.000000000000000000, -135.4552959529999896 ) ) ;
#16959 = ORIENTED_EDGE ( 'NONE', *, *, #22694, .T. ) ;
#16960 = DIRECTION ( 'NONE',  ( 1.000000000000000000, 0.000000000000000000, 0.000000000000000000 ) ) ;
#16961 = ORIENTED_EDGE ( 'NONE', *, *, #4435, .T. ) ;
#16962 = CARTESIAN_POINT ( 'NONE',  ( -6.384923429577490595, -17.86333053711281238, -143.5552959530020303 ) ) ;
#16963 = ORIENTED_EDGE ( 'NONE', *, *, #8488, .F. ) ;
#16964 = CARTESIAN_POINT ( 'NONE',  ( -27.58120011020000106, 38.53525547130000461, -147.4183263870000076 ) ) ;
#16965 = ORIENTED_EDGE ( 'NONE', *, *, #3868, .F. ) ;
#16966 = CARTESIAN_POINT ( 'NONE',  ( -22.79119882237723616, 32.80244356386412363, -141.5899087428671521 ) ) ;
#16967 = VERTEX_POINT ( 'NONE', #11678 ) ;
#16968 = CARTESIAN_POINT ( 'NONE',  ( -12.07808196999504879, -43.78524365307782062, -150.0552959529999555 ) ) ;
#16969 = ORIENTED_EDGE ( 'NONE', *, *, #14309, .F. ) ;
#16970 = ORIENTED_EDGE ( 'NONE', *, *, #16736, .F. ) ;
#16971 = LINE ( 'NONE', #11368, #20899 ) ;
#16972 = DIRECTION ( 'NONE',  ( -0.1435602414469281940, -0.9896415801065048257, 3.836930773098079160E-13 ) ) ;
#16973 = EDGE_CURVE ( 'NONE', #8373, #9593, #20514, .T. ) ;
#16974 = AXIS2_PLACEMENT_3D ( 'NONE', #2255, #14862, #6363 ) ;
#16975 = CARTESIAN_POINT ( 'NONE',  ( 4.500000000000000000, -3.500000000000000000, -145.5552959529999839 ) ) ;
#16976 = DIRECTION ( 'NONE',  ( 1.000000000000000000, 0.000000000000000000, -2.257157423930000049E-12 ) ) ;
#16977 = LINE ( 'NONE', #7695, #13304 ) ;
#16978 = CARTESIAN_POINT ( 'NONE',  ( -8.371159465364423014, 37.93364697496366489, -139.4097093116685073 ) ) ;
#16979 = ORIENTED_EDGE ( 'NONE', *, *, #8364, .F. ) ;
#16980 = DIRECTION ( 'NONE',  ( 0.000000000000000000, 0.000000000000000000, 1.000000000000000000 ) ) ;
#16981 = CARTESIAN_POINT ( 'NONE',  ( 9.487902780448600026, 38.13315664843509012, -146.2851006690217162 ) ) ;
#16982 = CARTESIAN_POINT ( 'NONE',  ( -26.61369313923911761, 36.92937183404333723, -140.1328975134356369 ) ) ;
#16983 = VERTEX_POINT ( 'NONE', #15387 ) ;
#16984 = VECTOR ( 'NONE', #7896, 1000.000000000000000 ) ;
#16985 = CARTESIAN_POINT ( 'NONE',  ( -12.18289575740000075, 37.87223172089999679, -148.4976681630000144 ) ) ;
#16986 = LINE ( 'NONE', #6163, #2950 ) ;
#16987 = FACE_OUTER_BOUND ( 'NONE', #3647, .T. ) ;
#16988 = VECTOR ( 'NONE', #16932, 1000.000000000000000 ) ;
#16989 = ORIENTED_EDGE ( 'NONE', *, *, #22924, .T. ) ;
#16990 = CARTESIAN_POINT ( 'NONE',  ( -7.015833805750000707, 33.30032478630000270, -141.9582197170000200 ) ) ;
#16991 = CARTESIAN_POINT ( 'NONE',  ( 3.611688725869999975E-11, -51.50000000000000000, -136.0552959530000123 ) ) ;
#16992 = ORIENTED_EDGE ( 'NONE', *, *, #16157, .T. ) ;
#16993 = CARTESIAN_POINT ( 'NONE',  ( -21.03694116389999635, 36.94210036639999828, -147.9486865819999935 ) ) ;
#16994 = FACE_OUTER_BOUND ( 'NONE', #9496, .T. ) ;
#16995 = EDGE_LOOP ( 'NONE', ( #20485, #10232, #22807, #20727 ) ) ;
#16996 = CARTESIAN_POINT ( 'NONE',  ( -3.500000000000000000, 46.50000000000000000, -150.0552959529999839 ) ) ;
#16997 = CARTESIAN_POINT ( 'NONE',  ( -20.60427366044887521, 39.77066172006404798, -140.2727996545226858 ) ) ;
#16998 = ORIENTED_EDGE ( 'NONE', *, *, #792, .T. ) ;
#16999 = CARTESIAN_POINT ( 'NONE',  ( -27.66848331343965128, 32.56468501992201681, -144.4027908766657902 ) ) ;
#17000 = CARTESIAN_POINT ( 'NONE',  ( -15.00000000000000000, -43.00000000000000000, -145.5552959529999839 ) ) ;
#17001 = EDGE_CURVE ( 'NONE', #16420, #22568, #15504, .T. ) ;
#17002 = ORIENTED_EDGE ( 'NONE', *, *, #21985, .T. ) ;
#17003 = DIRECTION ( 'NONE',  ( 1.000000000000000000, 0.000000000000000000, -2.257453483404485235E-12 ) ) ;
#17004 = CARTESIAN_POINT ( 'NONE',  ( 25.18320006080000084, -34.50000000000000000, -150.0552959529999839 ) ) ;
#17005 = CARTESIAN_POINT ( 'NONE',  ( -35.20609992760000040, 11.31289830180000067, -144.5552959529999839 ) ) ;
#17006 = AXIS2_PLACEMENT_3D ( 'NONE', #8470, #23233, #19787 ) ;
#17007 = VERTEX_POINT ( 'NONE', #13241 ) ;
#17008 = CARTESIAN_POINT ( 'NONE',  ( -20.54812748657685972, 36.93719815735425271, -140.4704715740689949 ) ) ;
#17009 = AXIS2_PLACEMENT_3D ( 'NONE', #19760, #9017, #15945 ) ;
#17010 = CARTESIAN_POINT ( 'NONE',  ( 27.68320006080000084, -32.50000000000000000, -150.0552959529999839 ) ) ;
#17011 = ORIENTED_EDGE ( 'NONE', *, *, #10335, .T. ) ;
#17012 = ORIENTED_EDGE ( 'NONE', *, *, #3400, .T. ) ;
#17013 = CARTESIAN_POINT ( 'NONE',  ( 3.714756346922155839, -0.5780819699950539015, -150.0552959529999839 ) ) ;
#17014 = CARTESIAN_POINT ( 'NONE',  ( 1.000000000140000012, 36.50000000000000000, -146.5552959529999839 ) ) ;
#17015 = CYLINDRICAL_SURFACE ( 'NONE', #9766, 1.500000000000001332 ) ;
#17016 = DIRECTION ( 'NONE',  ( -0.1743118874569385135, -0.9846904924346531196, 6.644571628977660906E-13 ) ) ;
#17017 = ORIENTED_EDGE ( 'NONE', *, *, #4547, .T. ) ;
#17018 = CARTESIAN_POINT ( 'NONE',  ( 4.500000000009999113, -3.500000000000000000, -137.0552959530000123 ) ) ;
#17019 = CARTESIAN_POINT ( 'NONE',  ( 1.759100530420000030, -16.38142836440000139, -143.0552959529999839 ) ) ;
#17020 = AXIS2_PLACEMENT_3D ( 'NONE', #16798, #5730, #18708 ) ;
#17021 = FACE_OUTER_BOUND ( 'NONE', #17824, .T. ) ;
#17022 = CARTESIAN_POINT ( 'NONE',  ( -34.50000000000000000, 76.00000000000000000, -155.5552959529999839 ) ) ;
#17023 = CARTESIAN_POINT ( 'NONE',  ( -24.68730002459999895, 39.33688142210000649, -147.2285014869999884 ) ) ;
#17024 = VECTOR ( 'NONE', #23175, 1000.000000000000000 ) ;
#17025 = CARTESIAN_POINT ( 'NONE',  ( -14.95010530348893951, 36.06328527009492291, -147.9474140018595563 ) ) ;
#17026 = EDGE_CURVE ( 'NONE', #4889, #18609, #890, .T. ) ;
#17027 = CARTESIAN_POINT ( 'NONE',  ( -16.46027398316528334, 32.88080821139473642, -146.2791150315001403 ) ) ;
#17028 = CARTESIAN_POINT ( 'NONE',  ( 5.276897646260000130, -21.39828525539999760, -144.5552959529999839 ) ) ;
#17029 = CYLINDRICAL_SURFACE ( 'NONE', #20223, 2.999999999999999112 ) ;
#17030 = ADVANCED_FACE ( 'NONE', ( #2325 ), #2787, .F. ) ;
#17031 = CARTESIAN_POINT ( 'NONE',  ( -6.049191701419999845, -14.51144913589999952, -145.5552959529999839 ) ) ;
#17032 = VERTEX_POINT ( 'NONE', #13595 ) ;
#17033 = CARTESIAN_POINT ( 'NONE',  ( -9.036966863464655830, 36.06754287650300483, -147.9517351211478342 ) ) ;
#17034 = LINE ( 'NONE', #13350, #21394 ) ;
#17035 = ORIENTED_EDGE ( 'NONE', *, *, #14940, .F. ) ;
#17036 = SURFACE_SIDE_STYLE ('',( #22747 ) ) ;
#17037 = AXIS2_PLACEMENT_3D ( 'NONE', #20851, #6325, #7329 ) ;
#17038 = AXIS2_PLACEMENT_3D ( 'NONE', #14637, #3335, #16427 ) ;
#17039 = CARTESIAN_POINT ( 'NONE',  ( -21.84945680779619437, 33.33324089315806305, -143.5473053630374523 ) ) ;
#17040 = PLANE ( 'NONE',  #16684 ) ;
#17041 = ORIENTED_EDGE ( 'NONE', *, *, #17495, .T. ) ;
#17042 = CARTESIAN_POINT ( 'NONE',  ( -12.86016529631691974, 36.30837334280015227, -147.6243440206422122 ) ) ;
#17043 = LINE ( 'NONE', #4326, #7814 ) ;
#17044 = VECTOR ( 'NONE', #18190, 1000.000000000000227 ) ;
#17045 = DIRECTION ( 'NONE',  ( -2.602084747549999882E-17, 1.000000000000000000, 5.873289694040000105E-29 ) ) ;
#17046 = CARTESIAN_POINT ( 'NONE',  ( -13.50000000000000000, -43.00000000000000000, -136.5552959530000123 ) ) ;
#17047 = LINE ( 'NONE', #15151, #5136 ) ;
#17048 = EDGE_CURVE ( 'NONE', #7777, #19702, #534, .T. ) ;
#17049 = CARTESIAN_POINT ( 'NONE',  ( -8.199334625101119656, 37.67958715123329938, -140.7360079146043290 ) ) ;
#17050 = ORIENTED_EDGE ( 'NONE', *, *, #22849, .F. ) ;
#17051 = CARTESIAN_POINT ( 'NONE',  ( -27.97684248819999908, 35.51254237909999745, -147.4365014880000047 ) ) ;
#17052 = AXIS2_PLACEMENT_3D ( 'NONE', #11379, #2133, #2594 ) ;
#17053 = VECTOR ( 'NONE', #20906, 1000.000000000000000 ) ;
#17054 = ORIENTED_EDGE ( 'NONE', *, *, #8631, .T. ) ;
#17055 = CARTESIAN_POINT ( 'NONE',  ( -13.33045527085381998, 32.30799570172891322, -144.7412170606758650 ) ) ;
#17056 = CARTESIAN_POINT ( 'NONE',  ( -34.50000000000000000, -74.00000000000000000, -132.5552959530000123 ) ) ;
#17057 = EDGE_CURVE ( 'NONE', #6997, #7250, #18732, .T. ) ;
#17058 = LINE ( 'NONE', #22192, #18408 ) ;
#17059 = VECTOR ( 'NONE', #23505, 999.9999999999998863 ) ;
#17060 = ORIENTED_EDGE ( 'NONE', *, *, #3419, .F. ) ;
#17061 = VECTOR ( 'NONE', #19716, 1000.000000000000000 ) ;
#17062 = DIRECTION ( 'NONE',  ( 1.000000000000000000, 2.004714280773594901E-17, -1.095180403012019938E-17 ) ) ;
#17063 = DIRECTION ( 'NONE',  ( -0.09606172499277226828, -0.9953753789357124848, 8.265980492677616040E-13 ) ) ;
#17064 = ORIENTED_EDGE ( 'NONE', *, *, #15610, .F. ) ;
#17065 = CARTESIAN_POINT ( 'NONE',  ( -20.97542662470000252, 40.85881720449999932, -141.8340754020000247 ) ) ;
#17066 = EDGE_CURVE ( 'NONE', #15585, #14843, #2442, .T. ) ;
#17067 = CARTESIAN_POINT ( 'NONE',  ( -18.85038775884696705, 39.40085191981486901, -147.1529297763815691 ) ) ;
#17068 = LINE ( 'NONE', #22554, #4931 ) ;
#17069 = VECTOR ( 'NONE', #12092, 1000.000000000000227 ) ;
#17070 = CARTESIAN_POINT ( 'NONE',  ( -9.056357402059999728, -12.43025388040000045, -146.5552959529999839 ) ) ;
#17071 = AXIS2_PLACEMENT_3D ( 'NONE', #12861, #18352, #16553 ) ;
#17072 = CARTESIAN_POINT ( 'NONE',  ( -24.73433384546525104, 33.38239242349900593, -144.4107376024117002 ) ) ;
#17073 = ORIENTED_EDGE ( 'NONE', *, *, #513, .T. ) ;
#17074 = VECTOR ( 'NONE', #10298, 1000.000000000000114 ) ;
#17075 = ADVANCED_FACE ( 'NONE', ( #17290 ), #1002, .F. ) ;
#17076 = VECTOR ( 'NONE', #3577, 1000.000000000000000 ) ;
#17077 = VECTOR ( 'NONE', #1318, 1000.000000000000000 ) ;
#17078 = EDGE_CURVE ( 'NONE', #6741, #9077, #18839, .T. ) ;
#17079 = CARTESIAN_POINT ( 'NONE',  ( -15.50000000000000000, 21.50000000000000000, -150.5552959529999839 ) ) ;
#17080 = ORIENTED_EDGE ( 'NONE', *, *, #387, .F. ) ;
#17081 = FACE_OUTER_BOUND ( 'NONE', #12897, .T. ) ;
#17082 = EDGE_CURVE ( 'NONE', #11018, #15585, #10829, .T. ) ;
#17083 = ORIENTED_EDGE ( 'NONE', *, *, #22749, .F. ) ;
#17084 = DIRECTION ( 'NONE',  ( 0.000000000000000000, 0.000000000000000000, 1.000000000000000000 ) ) ;
#17085 = VERTEX_POINT ( 'NONE', #17405 ) ;
#17086 = CARTESIAN_POINT ( 'NONE',  ( -6.370493725020000220, -17.65251768590000125, -145.5552959529999839 ) ) ;
#17087 = EDGE_CURVE ( 'NONE', #19419, #17813, #18258, .T. ) ;
#17088 = ORIENTED_EDGE ( 'NONE', *, *, #4815, .F. ) ;
#17089 = CARTESIAN_POINT ( 'NONE',  ( -0.009371101328294257835, 24.25767361204308870, -136.0552959530000123 ) ) ;
#17090 = VERTEX_POINT ( 'NONE', #4798 ) ;
#17091 = EDGE_LOOP ( 'NONE', ( #10750, #3649 ) ) ;
#17092 = LINE ( 'NONE', #809, #8708 ) ;
#17093 = CARTESIAN_POINT ( 'NONE',  ( -9.394779979509999990, -17.86685386420000299, -143.5552959529999839 ) ) ;
#17094 = CARTESIAN_POINT ( 'NONE',  ( -11.19806794730000021, 41.07225940149999843, -141.8826665010000170 ) ) ;
#17095 = VECTOR ( 'NONE', #1262, 1000.000000000000000 ) ;
#17096 = VECTOR ( 'NONE', #16713, 1000.000000000000000 ) ;
#17097 = CARTESIAN_POINT ( 'NONE',  ( 22.68320006080000084, -34.50000000000000000, -150.0552959529999839 ) ) ;
#17098 = AXIS2_PLACEMENT_3D ( 'NONE', #15776, #6610, #2584 ) ;
#17099 = CARTESIAN_POINT ( 'NONE',  ( -8.897765304693569632, 39.73354477844125654, -147.8293186649044912 ) ) ;
#17100 = AXIS2_PLACEMENT_3D ( 'NONE', #10207, #6409, #12235 ) ;
#17101 = ORIENTED_EDGE ( 'NONE', *, *, #98, .T. ) ;
#17102 = CARTESIAN_POINT ( 'NONE',  ( -22.10824191589999899, -32.00000000000000000, -150.0657682190000060 ) ) ;
#17103 = DIRECTION ( 'NONE',  ( 1.000000000000000000, 0.000000000000000000, 0.000000000000000000 ) ) ;
#17104 = CARTESIAN_POINT ( 'NONE',  ( -6.599319970649999867, -19.98386714700000155, -145.5552959529999839 ) ) ;
#17105 = EDGE_LOOP ( 'NONE', ( #8055, #4576, #2208, #9110, #17011, #3827, #9881, #14310, #8609, #13546 ) ) ;
#17106 = EDGE_CURVE ( 'NONE', #17493, #4135, #21224, .T. ) ;
#17107 = EDGE_CURVE ( 'NONE', #15489, #21292, #12041, .T. ) ;
#17108 = PLANE ( 'NONE',  #4848 ) ;
#17109 = CARTESIAN_POINT ( 'NONE',  ( 27.18320006080000084, 3.500000000000000000, -150.0552959529999839 ) ) ;
#17110 = EDGE_LOOP ( 'NONE', ( #6097, #16297, #20252, #23529, #15454, #22698, #16164 ) ) ;
#17111 = DIRECTION ( 'NONE',  ( 1.000000000000000000, 0.000000000000000000, 0.000000000000000000 ) ) ;
#17112 = CARTESIAN_POINT ( 'NONE',  ( 16.64676602990000021, -18.64223989710000140, -143.5552959529999839 ) ) ;
#17113 = VECTOR ( 'NONE', #13691, 1000.000000000000000 ) ;
#17114 = VECTOR ( 'NONE', #8516, 1000.000000000000000 ) ;
#17115 = EDGE_LOOP ( 'NONE', ( #17352, #14871, #13506, #3182 ) ) ;
#17116 = FACE_OUTER_BOUND ( 'NONE', #20418, .T. ) ;
#17117 = CYLINDRICAL_SURFACE ( 'NONE', #16051, 2.999999999999999112 ) ;
#17118 = VERTEX_POINT ( 'NONE', #10130 ) ;
#17119 = CARTESIAN_POINT ( 'NONE',  ( -14.12781175210000129, 38.88127384660000274, -139.8125553750000165 ) ) ;
#17120 = CARTESIAN_POINT ( 'NONE',  ( -20.65692115970000131, 38.75897267589999728, -140.0270467099999792 ) ) ;
#17121 = ORIENTED_EDGE ( 'NONE', *, *, #20371, .F. ) ;
#17122 = CARTESIAN_POINT ( 'NONE',  ( -28.70612892858435927, 35.15950212974924227, -139.8035036602273919 ) ) ;
#17123 = DIRECTION ( 'NONE',  ( 2.507771768019999718E-12, 1.592654864069999939E-17, -1.000000000000000000 ) ) ;
#17124 = ORIENTED_EDGE ( 'NONE', *, *, #16106, .F. ) ;
#17125 = PLANE ( 'NONE',  #21254 ) ;
#17126 = FACE_OUTER_BOUND ( 'NONE', #20411, .T. ) ;
#17127 = ORIENTED_EDGE ( 'NONE', *, *, #7490, .F. ) ;
#17128 = DIRECTION ( 'NONE',  ( 1.000000000000000000, 2.004714280773594901E-17, -1.095180403012019938E-17 ) ) ;
#17129 = ORIENTED_EDGE ( 'NONE', *, *, #5575, .F. ) ;
#17130 = CARTESIAN_POINT ( 'NONE',  ( 1.342750202250000191, -63.28208324180000233, -144.5552959529999839 ) ) ;
#17131 = CARTESIAN_POINT ( 'NONE',  ( -16.50000000000000000, -43.00000000000000000, -136.0552959530000123 ) ) ;
#17132 = ORIENTED_EDGE ( 'NONE', *, *, #374, .F. ) ;
#17133 = VECTOR ( 'NONE', #9648, 1000.000000000000000 ) ;
#17134 = ORIENTED_EDGE ( 'NONE', *, *, #16076, .T. ) ;
#17135 = PLANE ( 'NONE',  #17334 ) ;
#17136 = EDGE_CURVE ( 'NONE', #2114, #3418, #8580, .T. ) ;
#17137 = CARTESIAN_POINT ( 'NONE',  ( -32.50000000000000000, 48.00000000000000000, -137.5552959530000123 ) ) ;
#17138 = ADVANCED_FACE ( 'NONE', ( #8357, #14193 ), #3024, .T. ) ;
#17139 = FACE_OUTER_BOUND ( 'NONE', #521, .T. ) ;
#17140 = PLANE ( 'NONE',  #1900 ) ;
#17141 = ORIENTED_EDGE ( 'NONE', *, *, #6933, .F. ) ;
#17142 = CARTESIAN_POINT ( 'NONE',  ( -4.499999999959999109, 34.00000000000000000, -153.0552959529999839 ) ) ;
#17143 = CARTESIAN_POINT ( 'NONE',  ( -7.500000000000000000, 25.50000000000000000, -150.5552959529999839 ) ) ;
#17144 = DIRECTION ( 'NONE',  ( 0.9968185442904002880, -0.07970438983373201447, -8.712538262633510059E-14 ) ) ;
#17145 = CARTESIAN_POINT ( 'NONE',  ( -30.97299999999999898, 14.00000000000000000, -144.0552959529999839 ) ) ;
#17146 = CARTESIAN_POINT ( 'NONE',  ( -24.39610112286784371, 41.30434740782117586, -144.5132185276669929 ) ) ;
#17147 = CLOSED_SHELL ( 'NONE', ( #11212, #11696, #20477, #21439, #20733, #6015, #16074, #11534, #16475, #1558, #21782, #18626, #12156, #13792, #11480, #1923, #14765, #15392, #2723, #15674, #4312, #3412, #14993, #7726, #10621, #4136, #1339, #12515, #22064, #9793, #12427, #12005, #15476, #3420, #11248, #18834, #22004, #9388, #21043, #12027, #2286, #7744, #7487, #14043, #23277, #9899, #21464, #2141, #1362, #20374, #14785, #4289, #9227, #13590, #6074, #16845, #15917, #15298, #19051, #15752, #5776, #23471, #10373, #1703, #1033, #20452, #2430, #1937, #5873, #15349, #14020, #7363, #10387, #6333, #6335, #21756, #9034, #8599, #11747, #13846 ) ) ;
#17148 = VECTOR ( 'NONE', #17735, 1000.000000000000000 ) ;
#17149 = CARTESIAN_POINT ( 'NONE',  ( -15.99498317667975122, 33.76443601943795869, -141.9451672683316872 ) ) ;
#17150 = CARTESIAN_POINT ( 'NONE',  ( -16.46770182039374220, 34.68366497520294445, -147.1680949295432583 ) ) ;
#17151 = CARTESIAN_POINT ( 'NONE',  ( 1.847645635000000119, -15.93876195360000025, -145.5552959529999839 ) ) ;
#17152 = DIRECTION ( 'NONE',  ( 1.000000000000000000, 0.000000000000000000, 2.516505522483685870E-12 ) ) ;
#17153 = LINE ( 'NONE', #11659, #1699 ) ;
#17154 = ORIENTED_EDGE ( 'NONE', *, *, #15047, .T. ) ;
#17155 = CARTESIAN_POINT ( 'NONE',  ( -9.784659724394936475, 33.29695882288061171, -143.3891222208823422 ) ) ;
#17156 = DIRECTION ( 'NONE',  ( 1.000000000000000000, 0.000000000000000000, -1.522591576628786004E-13 ) ) ;
#17157 = FACE_OUTER_BOUND ( 'NONE', #376, .T. ) ;
#17158 = EDGE_LOOP ( 'NONE', ( #13073, #6213, #19909, #13411 ) ) ;
#17159 = CYLINDRICAL_SURFACE ( 'NONE', #12185, 3.500000000000000000 ) ;
#17160 = CARTESIAN_POINT ( 'NONE',  ( -21.32007872946885030, 35.46309690574533846, -147.3430777018452602 ) ) ;
#17161 = VECTOR ( 'NONE', #21199, 1000.000000000000000 ) ;
#17162 = VECTOR ( 'NONE', #3847, 1000.000000000000000 ) ;
#17163 = DIRECTION ( 'NONE',  ( 4.510170015240000199E-12, -1.314504061159999897E-13, 1.000000000000000000 ) ) ;
#17164 = EDGE_LOOP ( 'NONE', ( #13633, #16059, #11367, #21705 ) ) ;
#17165 = VECTOR ( 'NONE', #12784, 1000.000000000000000 ) ;
#17166 = CARTESIAN_POINT ( 'NONE',  ( -23.51619327739999932, 36.94101002280000046, -140.1031831869999849 ) ) ;
#17167 = EDGE_CURVE ( 'NONE', #5668, #15811, #21345, .T. ) ;
#17168 = CARTESIAN_POINT ( 'NONE',  ( 0.3832000607639999834, -34.50000000000000000, -149.3052959529999839 ) ) ;
#17169 = CARTESIAN_POINT ( 'NONE',  ( 1.544882029667944634, 14.84887268567880270, -150.0552959529999839 ) ) ;
#17170 = CARTESIAN_POINT ( 'NONE',  ( 6.499999999879999102, -3.000000000000000000, -135.0552959530000123 ) ) ;
#17171 = PLANE ( 'NONE',  #661 ) ;
#17172 = ADVANCED_FACE ( 'NONE', ( #15741 ), #15853, .F. ) ;
#17173 = LINE ( 'NONE', #15031, #1367 ) ;
#17174 = CARTESIAN_POINT ( 'NONE',  ( 8.976561295253542738, -38.03342539458719074, -150.0552959529999555 ) ) ;
#17175 = ORIENTED_EDGE ( 'NONE', *, *, #10824, .F. ) ;
#17176 = CARTESIAN_POINT ( 'NONE',  ( 6.500000000170000014, 20.50000000000000000, -136.5552959530000123 ) ) ;
#17177 = SHAPE_REPRESENTATION_RELATIONSHIP ( 'NONE' , 'NONE' ,  #23186, #10046 ) ;
#17178 = ORIENTED_EDGE ( 'NONE', *, *, #14608, .F. ) ;
#17179 = CARTESIAN_POINT ( 'NONE',  ( -13.84608127647538289, 33.21776854254977707, -143.8496330080570829 ) ) ;
#17180 = VECTOR ( 'NONE', #1229, 1000.000000000000000 ) ;
#17181 = CARTESIAN_POINT ( 'NONE',  ( 18.95053822279999878, 50.00000000000000000, -150.0552959529999839 ) ) ;
#17182 = CIRCLE ( 'NONE', #9945, 0.5000000000000009992 ) ;
#17183 = B_SPLINE_CURVE_WITH_KNOTS ( 'NONE', 3,
 ( #11715, #19223, #20781, #10292, #10044, #1036, #17089, #1165, #13986, #2932, #4596, #21144, #15539, #17441, #1282, #8266, #2704, #11839 ),
 .UNSPECIFIED., .F., .F.,
 ( 4, 2, 2, 2, 2, 2, 2, 2, 4 ),
 ( 0.000000000000000000, 0.1250000000000000278, 0.2500000000000000555, 0.3750000000000001110, 0.5000000000000001110, 0.6250000000000001110, 0.7500000000000002220, 0.8750000000000001110, 1.000000000000000000 ),
 .UNSPECIFIED. ) ;
#17184 = ORIENTED_EDGE ( 'NONE', *, *, #23226, .T. ) ;
#17185 = DIRECTION ( 'NONE',  ( 1.000000000000000000, 0.000000000000000000, 0.000000000000000000 ) ) ;
#17186 = DIRECTION ( 'NONE',  ( -1.000000000000000000, 5.094701932209999624E-24, 0.000000000000000000 ) ) ;
#17187 = ORIENTED_EDGE ( 'NONE', *, *, #4894, .T. ) ;
#17188 = FACE_OUTER_BOUND ( 'NONE', #15443, .T. ) ;
#17189 = CARTESIAN_POINT ( 'NONE',  ( -17.65545014875934626, 37.67134846496733758, -140.4683765912815545 ) ) ;
#17190 = CARTESIAN_POINT ( 'NONE',  ( 7.229469229562214494, 37.79933614746168757, -146.4244424236882480 ) ) ;
#17191 = FACE_OUTER_BOUND ( 'NONE', #4000, .T. ) ;
#17192 = CARTESIAN_POINT ( 'NONE',  ( -25.26464694443967929, 35.54252112450230783, -140.6256209330285287 ) ) ;
#17193 = CARTESIAN_POINT ( 'NONE',  ( 3.000000000000000000, -3.500000000000000000, -150.0552959529999839 ) ) ;
#17194 = ADVANCED_FACE ( 'NONE', ( #12163 ), #21458, .T. ) ;
#17195 = AXIS2_PLACEMENT_3D ( 'NONE', #20383, #16379, #8102 ) ;
#17196 = ORIENTED_EDGE ( 'NONE', *, *, #17344, .F. ) ;
#17197 = LINE ( 'NONE', #9802, #7524 ) ;
#17198 = ORIENTED_EDGE ( 'NONE', *, *, #20568, .T. ) ;
#17199 = LINE ( 'NONE', #11591, #94 ) ;
#17200 = ORIENTED_EDGE ( 'NONE', *, *, #5032, .T. ) ;
#17201 = CARTESIAN_POINT ( 'NONE',  ( -13.86630785140000022, 50.99999999970000175, -136.0552959530000123 ) ) ;
#17202 = ADVANCED_FACE ( 'NONE', ( #5139 ), #4632, .F. ) ;
#17203 = ORIENTED_EDGE ( 'NONE', *, *, #17167, .T. ) ;
#17204 = DIRECTION ( 'NONE',  ( 2.255973186040000320E-12, 0.000000000000000000, 1.000000000000000000 ) ) ;
#17205 = ORIENTED_EDGE ( 'NONE', *, *, #4295, .T. ) ;
#17206 = ORIENTED_EDGE ( 'NONE', *, *, #19294, .F. ) ;
#17207 = FACE_OUTER_BOUND ( 'NONE', #7613, .T. ) ;
#17208 = LINE ( 'NONE', #4252, #15572 ) ;
#17209 = CARTESIAN_POINT ( 'NONE',  ( -10.95384970519167034, 40.87632101822132569, -142.0199864900084208 ) ) ;
#17210 = STYLED_ITEM ( 'NONE', ( #18902 ), #23143 ) ;
#17211 = DIRECTION ( 'NONE',  ( 2.257144641399999941E-12, -4.009147065136860232E-51, 1.000000000000000000 ) ) ;
#17212 = CARTESIAN_POINT ( 'NONE',  ( -21.35824191589999899, -4.750000000000000000, -145.5657682190000060 ) ) ;
#17213 = EDGE_CURVE ( 'NONE', #9023, #5742, #22043, .T. ) ;
#17214 = CARTESIAN_POINT ( 'NONE',  ( -8.441146697811769073, 41.59278767816196876, -144.5480507108394477 ) ) ;
#17215 = VERTEX_POINT ( 'NONE', #11300 ) ;
#17216 = DIRECTION ( 'NONE',  ( 2.257144641399999941E-12, -8.049635416090000264E-35, 1.000000000000000000 ) ) ;
#17217 = EDGE_CURVE ( 'NONE', #17032, #16762, #19046, .T. ) ;
#17218 = CARTESIAN_POINT ( 'NONE',  ( 9.960532536797563452, 36.60272478500484539, -146.5309852632849470 ) ) ;
#17219 = CARTESIAN_POINT ( 'NONE',  ( -13.86630785130000021, -51.00000000000000000, -136.0552959530000123 ) ) ;
#17220 = ORIENTED_EDGE ( 'NONE', *, *, #15341, .F. ) ;
#17221 = DIRECTION ( 'NONE',  ( 0.000000000000000000, 0.000000000000000000, 1.000000000000000000 ) ) ;
#17222 = DIRECTION ( 'NONE',  ( 1.000000000000000000, 0.000000000000000000, 0.000000000000000000 ) ) ;
#17223 = ORIENTED_EDGE ( 'NONE', *, *, #14345, .F. ) ;
#17224 = LINE ( 'NONE', #2955, #13201 ) ;
#17225 = COLOUR_RGB ( '', 0.31764706, 0.68627451, 0.89019608) ;
#17226 = DIRECTION ( 'NONE',  ( 1.000000000000000000, 0.000000000000000000, -2.259525899719999991E-12 ) ) ;
#17227 = ORIENTED_EDGE ( 'NONE', *, *, #4515, .T. ) ;
#17228 = CARTESIAN_POINT ( 'NONE',  ( -12.50000000000000000, 19.50000000000000000, -137.0552959530000123 ) ) ;
#17229 = CARTESIAN_POINT ( 'NONE',  ( 20.50000000000000355, -20.89269908169873347, -150.0552959530000123 ) ) ;
#17230 = VERTEX_POINT ( 'NONE', #2523 ) ;
#17231 = AXIS2_PLACEMENT_3D ( 'NONE', #20185, #7543, #10999 ) ;
#17232 = CARTESIAN_POINT ( 'NONE',  ( -15.02010258789212926, 41.63949583921710484, -143.5015232158323499 ) ) ;
#17233 = APPLICATION_CONTEXT ( 'automotive_design' ) ;
#17234 = EDGE_CURVE ( 'NONE', #3138, #21821, #9521, .T. ) ;
#17235 = CARTESIAN_POINT ( 'NONE',  ( -26.29566636579999894, 36.18167175180000328, -140.3932108110000172 ) ) ;
#17236 = ORIENTED_EDGE ( 'NONE', *, *, #22546, .F. ) ;
#17237 =( LENGTH_UNIT ( ) NAMED_UNIT ( * ) SI_UNIT ( .MILLI., .METRE. ) );
#17238 = EDGE_CURVE ( 'NONE', #5977, #20549, #6086, .T. ) ;
#17240 = CARTESIAN_POINT ( 'NONE',  ( -18.35824191589999899, -34.50000000000000000, -146.3157682190000060 ) ) ;
#17239 = B_SPLINE_CURVE_WITH_KNOTS ( 'NONE', 3,
 ( #14925, #22182, #5868, #13126, #18608, #10263, #13842, #15630, #4563, #1128, #6578, #22895, #8358, #3026, #2901, #13365, #11803, #13723, #17291, #9773, #6342, #1003, #15742, #21109, #19080, #15506, #17530, #4330, #2670, #10132, #4799, #12043, #17174, #13596 ),
 .UNSPECIFIED., .F., .F.,
 ( 4, 2, 2, 2, 2, 2, 2, 2, 2, 2, 2, 2, 2, 2, 2, 2, 4 ),
 ( 0.000000000000000000, 0.06250000000000004163, 0.1250000000000000833, 0.1875000000000001943, 0.2500000000000002776, 0.3125000000000003331, 0.3750000000000003886, 0.4375000000000003886, 0.5000000000000004441, 0.5625000000000004441, 0.6250000000000004441, 0.6875000000000003331, 0.7500000000000002220, 0.8125000000000002220, 0.8750000000000001110, 0.9375000000000001110, 1.000000000000000000 ),
 .UNSPECIFIED. ) ;
#17241 = EDGE_LOOP ( 'NONE', ( #22284, #5418, #2036, #8064 ) ) ;
#17242 = CARTESIAN_POINT ( 'NONE',  ( -34.47299999999999898, 14.00000000000000000, -144.0552959529999839 ) ) ;
#17243 = DIRECTION ( 'NONE',  ( -1.296824736026760017E-11, 0.000000000000000000, 1.000000000000000000 ) ) ;
#17244 = ORIENTED_EDGE ( 'NONE', *, *, #2419, .F. ) ;
#17245 = CARTESIAN_POINT ( 'NONE',  ( -46.50000000000000000, 47.50000000000000000, -148.7506583580000097 ) ) ;
#17246 = ORIENTED_EDGE ( 'NONE', *, *, #7210, .T. ) ;
#17247 = ADVANCED_FACE ( 'NONE', ( #15471 ), #7973, .F. ) ;
#17248 = DIRECTION ( 'NONE',  ( 1.000000000000000000, 0.000000000000000000, -1.701177084980000217E-20 ) ) ;
#17249 = ADVANCED_FACE ( 'NONE', ( #7851 ), #6200, .T. ) ;
#17250 = DIRECTION ( 'NONE',  ( -2.808280234689999718E-18, 1.000000000000000000, 1.592654863659999653E-17 ) ) ;
#17251 = ORIENTED_EDGE ( 'NONE', *, *, #11999, .F. ) ;
#17252 = ADVANCED_FACE ( 'NONE', ( #11649 ), #15249, .T. ) ;
#17253 = VECTOR ( 'NONE', #4928, 1000.000000000000000 ) ;
#17254 = EDGE_CURVE ( 'NONE', #8318, #8477, #13116, .T. ) ;
#17255 = ORIENTED_EDGE ( 'NONE', *, *, #2694, .T. ) ;
#17256 = CARTESIAN_POINT ( 'NONE',  ( -16.50000000000000000, -43.00000000000000000, -137.0552959530000123 ) ) ;
#17257 = CARTESIAN_POINT ( 'NONE',  ( -4.584402860569999127, 37.05223431090000474, -140.2914745300000163 ) ) ;
#17258 = CARTESIAN_POINT ( 'NONE',  ( 1.708387416626109934, -17.47608414525880960, -147.5552959529822488 ) ) ;
#17259 = CARTESIAN_POINT ( 'NONE',  ( -44.50000000000000000, 29.00000000000000000, -148.4460207619999892 ) ) ;
#17260 = ORIENTED_EDGE ( 'NONE', *, *, #6586, .F. ) ;
#17261 = CARTESIAN_POINT ( 'NONE',  ( 8.633772787779999902, -29.00605602609999778, -146.5552959529999839 ) ) ;
#17262 = DIRECTION ( 'NONE',  ( 0.000000000000000000, 1.000000000000000000, 0.000000000000000000 ) ) ;
#17263 = DIRECTION ( 'NONE',  ( -0.000000000000000000, 1.000000000000000000, 0.000000000000000000 ) ) ;
#17264 = PLANE ( 'NONE',  #18927 ) ;
#17265 = CARTESIAN_POINT ( 'NONE',  ( -25.85824191589999899, -13.50000000000000000, -144.8157682190000060 ) ) ;
#17266 = LINE ( 'NONE', #6783, #11704 ) ;
#17267 = ORIENTED_EDGE ( 'NONE', *, *, #2222, .T. ) ;
#17268 = DIRECTION ( 'NONE',  ( 1.000000000000000000, 0.000000000000000000, 0.000000000000000000 ) ) ;
#17269 = VECTOR ( 'NONE', #10354, 999.9999999999998863 ) ;
#17270 = CARTESIAN_POINT ( 'NONE',  ( -17.20894333738748117, 33.38229181965237302, -141.8650879853053368 ) ) ;
#17271 = CARTESIAN_POINT ( 'NONE',  ( 20.50000000000000000, -20.50000000000000000, -143.5552959529999839 ) ) ;
#17272 = LINE ( 'NONE', #10236, #3894 ) ;
#17273 = LINE ( 'NONE', #19418, #20317 ) ;
#17274 = EDGE_LOOP ( 'NONE', ( #14826, #19413, #2076, #20951 ) ) ;
#17275 = CARTESIAN_POINT ( 'NONE',  ( -9.874497313270580889, -24.62570111238803960, -143.5552959529987334 ) ) ;
#17276 = CARTESIAN_POINT ( 'NONE',  ( 23.50000000000000000, -20.50000000000000000, -137.2152959530000089 ) ) ;
#17277 = EDGE_CURVE ( 'NONE', #13352, #18640, #20715, .T. ) ;
#17278 = CARTESIAN_POINT ( 'NONE',  ( 5.419886383052536338, -2.299140194000087511, -150.0552959529999839 ) ) ;
#17279 = ORIENTED_EDGE ( 'NONE', *, *, #10028, .T. ) ;
#17280 = DIRECTION ( 'NONE',  ( 0.000000000000000000, 1.000000000000000000, 0.000000000000000000 ) ) ;
#17281 = DIRECTION ( 'NONE',  ( -1.000000000000000000, 0.000000000000000000, -2.245315044999999693E-12 ) ) ;
#17282 = LINE ( 'NONE', #6220, #8700 ) ;
#17283 = ORIENTED_EDGE ( 'NONE', *, *, #21016, .F. ) ;
#17284 = LINE ( 'NONE', #10364, #5291 ) ;
#17285 = PLANE ( 'NONE',  #22655 ) ;
#17286 = DIRECTION ( 'NONE',  ( 2.839308199618490134E-14, 3.568879590628495223E-13, 1.000000000000000000 ) ) ;
#17287 = DIRECTION ( 'NONE',  ( 0.8571428571427679444, 0.5150787536378610421, -1.934960128632415569E-12 ) ) ;
#17288 = VECTOR ( 'NONE', #5867, 1000.000000000000000 ) ;
#17289 = CARTESIAN_POINT ( 'NONE',  ( -9.285539185979999388, 35.09287230280000358, -147.9937876190000168 ) ) ;
#17290 = FACE_OUTER_BOUND ( 'NONE', #11785, .T. ) ;
#17291 = CARTESIAN_POINT ( 'NONE',  ( 7.351088731964408041, -33.04529868153298366, -150.0552959529999839 ) ) ;
#17292 = EDGE_LOOP ( 'NONE', ( #13667, #8485, #5297, #9353 ) ) ;
#17293 = SURFACE_SIDE_STYLE ('',( #4802 ) ) ;
#17294 = ORIENTED_EDGE ( 'NONE', *, *, #19864, .T. ) ;
#17295 = CARTESIAN_POINT ( 'NONE',  ( -7.010349701908019426, 37.05829245174740549, -148.1453878984958124 ) ) ;
#17296 = DIRECTION ( 'NONE',  ( 0.000000000000000000, 0.000000000000000000, -1.000000000000000000 ) ) ;
#17297 = CARTESIAN_POINT ( 'NONE',  ( -2.499999999929999994, 41.25000000000000000, -138.0552959530000123 ) ) ;
#17298 = EDGE_LOOP ( 'NONE', ( #15282, #10116, #20784, #13728, #451, #20210 ) ) ;
#17299 = EDGE_CURVE ( 'NONE', #2628, #2618, #18926, .T. ) ;
#17300 = CARTESIAN_POINT ( 'NONE',  ( 23.40529971389999986, -31.60139774330000151, -147.5552959529999839 ) ) ;
#17301 = CARTESIAN_POINT ( 'NONE',  ( -15.37212823710000009, 38.89807584180000077, -148.3010324070000081 ) ) ;
#17302 = AXIS2_PLACEMENT_3D ( 'NONE', #20607, #4530, #2300 ) ;
#17303 = EDGE_CURVE ( 'NONE', #23020, #7470, #15006, .T. ) ;
#17304 = VERTEX_POINT ( 'NONE', #20370 ) ;
#17305 = LINE ( 'NONE', #1019, #9510 ) ;
#17306 = CARTESIAN_POINT ( 'NONE',  ( -17.83048858051152408, 39.52908467829296768, -140.3990652861876072 ) ) ;
#17307 = CARTESIAN_POINT ( 'NONE',  ( -16.50000000000000000, -43.19873783136716128, -150.0552959530000123 ) ) ;
#17308 = CARTESIAN_POINT ( 'NONE',  ( 7.371865253256605577, 37.99344671901626214, -146.3507065507166658 ) ) ;
#17309 = DIRECTION ( 'NONE',  ( 2.257144641397284947E-12, 2.714724913984255017E-24, 1.000000000000000000 ) ) ;
#17310 = CARTESIAN_POINT ( 'NONE',  ( -24.97797643630000053, 37.05442817780000553, -147.8575004449999994 ) ) ;
#17311 = CARTESIAN_POINT ( 'NONE',  ( -38.72222222220000276, 45.00000000000000000, -140.5552959529999839 ) ) ;
#17312 = EDGE_LOOP ( 'NONE', ( #7908, #19348, #22569, #9927 ) ) ;
#17313 = VECTOR ( 'NONE', #19958, 1000.000000000000000 ) ;
#17314 = CARTESIAN_POINT ( 'NONE',  ( -15.00000000000000000, -43.00000000000000000, -140.0552959529999839 ) ) ;
#17315 = VECTOR ( 'NONE', #22204, 1000.000000000000000 ) ;
#17316 = PRODUCT_DEFINITION_CONTEXT ( 'detailed design', #13577, 'design' ) ;
#17317 = EDGE_LOOP ( 'NONE', ( #1557, #15961, #11705, #20390 ) ) ;
#17318 = ORIENTED_EDGE ( 'NONE', *, *, #8060, .F. ) ;
#17319 = CARTESIAN_POINT ( 'NONE',  ( 19.86977406280000125, -31.59375768830000197, -148.5552959529999839 ) ) ;
#17320 = ORIENTED_EDGE ( 'NONE', *, *, #8041, .T. ) ;
#17321 = LINE ( 'NONE', #6258, #10631 ) ;
#17322 = ORIENTED_EDGE ( 'NONE', *, *, #4482, .F. ) ;
#17323 = ORIENTED_EDGE ( 'NONE', *, *, #19945, .F. ) ;
#17324 = ADVANCED_FACE ( 'NONE', ( #4065 ), #22268, .F. ) ;
#17325 = CARTESIAN_POINT ( 'NONE',  ( 19.13369214859999801, -50.50000000000000000, -136.0552959530000123 ) ) ;
#17326 = CARTESIAN_POINT ( 'NONE',  ( -15.27002291899999875, 38.46844526379999962, -147.3668459620000135 ) ) ;
#17327 = DIRECTION ( 'NONE',  ( 1.000000000000000000, 0.000000000000000000, 2.504935852220000146E-12 ) ) ;
#17328 = EDGE_CURVE ( 'NONE', #12661, #14517, #15121, .T. ) ;
#17329 = CARTESIAN_POINT ( 'NONE',  ( -8.008464111580879674, 33.29536412579140148, -142.0809313905602096 ) ) ;
#17330 = CARTESIAN_POINT ( 'NONE',  ( -9.937276790871505838, 38.82225217169769849, -147.9475752953410392 ) ) ;
#17331 = ORIENTED_EDGE ( 'NONE', *, *, #5639, .T. ) ;
#17332 = CARTESIAN_POINT ( 'NONE',  ( -13.86630785130000021, -50.50000000000000000, -137.0552959530000123 ) ) ;
#17333 = PRODUCT_DEFINITION_SHAPE ( 'NONE', 'NONE',  #23553 ) ;
#17334 = AXIS2_PLACEMENT_3D ( 'NONE', #856, #8085, #22610 ) ;
#17335 = CIRCLE ( 'NONE', #18473, 9.999999999999998224 ) ;
#17336 = DIRECTION ( 'NONE',  ( 1.000000000000000000, 0.000000000000000000, 0.000000000000000000 ) ) ;
#17337 = FACE_OUTER_BOUND ( 'NONE', #17158, .T. ) ;
#17338 = ORIENTED_EDGE ( 'NONE', *, *, #11917, .F. ) ;
#17339 = DIRECTION ( 'NONE',  ( 4.430318231639999944E-12, -6.100259101500000139E-13, 1.000000000000000000 ) ) ;
#17340 = CARTESIAN_POINT ( 'NONE',  ( 6.500000000159999125, 20.50000000000000000, -140.0552959529999839 ) ) ;
#17341 = ORIENTED_EDGE ( 'NONE', *, *, #16238, .T. ) ;
#17342 = CARTESIAN_POINT ( 'NONE',  ( 10.50000000010000001, 16.50000000000000000, -143.5552959529999839 ) ) ;
#17343 = DIRECTION ( 'NONE',  ( 1.000000000000000000, 0.000000000000000000, -2.257171095940000041E-12 ) ) ;
#17344 = EDGE_CURVE ( 'NONE', #22716, #16508, #9633, .T. ) ;
#17345 = VERTEX_POINT ( 'NONE', #7739 ) ;
#17346 = CARTESIAN_POINT ( 'NONE',  ( 1.591914056710000080, -18.48847405160000079, -144.5552959529999839 ) ) ;
#17347 = CARTESIAN_POINT ( 'NONE',  ( 21.98914305888730780, -23.12135916506278122, -150.0552959529999839 ) ) ;
#17348 = ORIENTED_EDGE ( 'NONE', *, *, #4274, .F. ) ;
#17349 = CARTESIAN_POINT ( 'NONE',  ( -15.19793912339760134, 40.53066279750093770, -141.9083977990133860 ) ) ;
#17350 = VECTOR ( 'NONE', #14736, 1000.000000000000114 ) ;
#17351 = CARTESIAN_POINT ( 'NONE',  ( -25.40969612650229337, 34.57839653382308853, -147.5232836264007119 ) ) ;
#17352 = ORIENTED_EDGE ( 'NONE', *, *, #7784, .T. ) ;
#17353 = FACE_OUTER_BOUND ( 'NONE', #2739, .T. ) ;
#17354 = ORIENTED_EDGE ( 'NONE', *, *, #11164, .T. ) ;
#17355 = DIRECTION ( 'NONE',  ( -0.6459422414661291079, -0.7633862853691523176, -2.245315045000450442E-12 ) ) ;
#17356 = LINE ( 'NONE', #19742, #5421 ) ;
#17357 = VERTEX_POINT ( 'NONE', #18811 ) ;
#17358 = EDGE_CURVE ( 'NONE', #3155, #7827, #10853, .T. ) ;
#17359 = DIRECTION ( 'NONE',  ( 1.000000000000000000, 0.000000000000000000, 2.516505522483685870E-12 ) ) ;
#17360 = ORIENTED_EDGE ( 'NONE', *, *, #20164, .F. ) ;
#17361 = DIRECTION ( 'NONE',  ( 1.000000000000000000, 0.000000000000000000, 0.000000000000000000 ) ) ;
#17362 = DIRECTION ( 'NONE',  ( 0.4794255386042040601, 0.8775825618903723147, 0.000000000000000000 ) ) ;
#17363 = VERTEX_POINT ( 'NONE', #2987 ) ;
#17364 = VECTOR ( 'NONE', #12891, 1000.000000000000000 ) ;
#17365 = EDGE_CURVE ( 'NONE', #477, #14591, #3330, .T. ) ;
#17366 = AXIS2_PLACEMENT_3D ( 'NONE', #18115, #1951, #3482 ) ;
#17367 = ORIENTED_EDGE ( 'NONE', *, *, #7602, .T. ) ;
#17368 = CARTESIAN_POINT ( 'NONE',  ( -5.070907855429999778, -22.41528233759999722, -147.5552959529999839 ) ) ;
#17369 = DIRECTION ( 'NONE',  ( 1.000000000000000000, -5.094701932209999624E-24, 0.000000000000000000 ) ) ;
#17370 = DIRECTION ( 'NONE',  ( -2.257171095940000041E-12, 0.000000000000000000, -1.000000000000000000 ) ) ;
#17371 = CARTESIAN_POINT ( 'NONE',  ( -21.16189237505000875, -3.249999999999015454, -146.3157682189995512 ) ) ;
#17372 = EDGE_LOOP ( 'NONE', ( #20234, #22217, #21026, #9312 ) ) ;
#17373 = LINE ( 'NONE', #861, #20062 ) ;
#17374 = CARTESIAN_POINT ( 'NONE',  ( -32.50000000000000000, 19.50000000000000000, -149.5552959529999839 ) ) ;
#17375 = EDGE_CURVE ( 'NONE', #10456, #12686, #4652, .T. ) ;
#17376 = DIRECTION ( 'NONE',  ( 5.094701932209999624E-24, 1.000000000000000000, -1.149947916579999802E-35 ) ) ;
#17377 = CARTESIAN_POINT ( 'NONE',  ( -15.19857565926003673, -41.49993277010363357, -150.0552959530000123 ) ) ;
#17378 = PLANE ( 'NONE',  #16013 ) ;
#17379 = LINE ( 'NONE', #22980, #13229 ) ;
#17380 = EDGE_CURVE ( 'NONE', #4360, #6192, #3108, .T. ) ;
#17381 = ORIENTED_EDGE ( 'NONE', *, *, #9226, .T. ) ;
#17382 = PLANE ( 'NONE',  #14515 ) ;
#17383 = EDGE_CURVE ( 'NONE', #11841, #8740, #21312, .T. ) ;
#17384 = AXIS2_PLACEMENT_3D ( 'NONE', #16446, #12860, #382 ) ;
#17385 = DIRECTION ( 'NONE',  ( 0.000000000000000000, -1.000000000000000000, 8.159623473500000156E-13 ) ) ;
#17386 = EDGE_CURVE ( 'NONE', #19806, #10546, #5114, .T. ) ;
#17387 = CARTESIAN_POINT ( 'NONE',  ( 6.500000000170000014, 24.50000000000000000, -136.5552959530000123 ) ) ;
#17388 = DIRECTION ( 'NONE',  ( 3.494344380199214996E-12, 0.000000000000000000, -1.000000000000000000 ) ) ;
#17389 = DIRECTION ( 'NONE',  ( 0.000000000000000000, 0.000000000000000000, 1.000000000000000000 ) ) ;
#17390 = ORIENTED_EDGE ( 'NONE', *, *, #18941, .F. ) ;
#17391 = CARTESIAN_POINT ( 'NONE',  ( -10.67777851957104396, 33.99926051417099160, -142.1577009039073971 ) ) ;
#17392 = CARTESIAN_POINT ( 'NONE',  ( -9.434278515689999978, -18.41834002140000237, -146.5552959529999839 ) ) ;
#17393 = DIRECTION ( 'NONE',  ( 1.000000000000000000, 0.000000000000000000, -2.259525899719999991E-12 ) ) ;
#17394 = ORIENTED_EDGE ( 'NONE', *, *, #3416, .F. ) ;
#17395 = DIRECTION ( 'NONE',  ( 3.994014902950000436E-29, -1.000000000000000000, 4.148443855749999753E-27 ) ) ;
#17396 = CARTESIAN_POINT ( 'NONE',  ( -28.81652202475261859, 33.24392987422240253, -143.6567944639990628 ) ) ;
#17397 = DIRECTION ( 'NONE',  ( 2.257157423930000049E-12, 0.000000000000000000, 1.000000000000000000 ) ) ;
#17398 = ORIENTED_EDGE ( 'NONE', *, *, #5328, .T. ) ;
#17399 = CARTESIAN_POINT ( 'NONE',  ( -13.26119488862553553, 36.18558975636723574, -139.9165878528899327 ) ) ;
#17400 = AXIS2_PLACEMENT_3D ( 'NONE', #388, #7626, #22863 ) ;
#17401 = DIRECTION ( 'NONE',  ( 0.000000000000000000, 1.000000000000000000, 0.000000000000000000 ) ) ;
#17402 = FACE_OUTER_BOUND ( 'NONE', #11327, .T. ) ;
#17403 = CARTESIAN_POINT ( 'NONE',  ( 8.500000000060001781, 38.50000000000000000, -142.0552959529999839 ) ) ;
#17404 = CARTESIAN_POINT ( 'NONE',  ( -10.86833117931673875, 32.45440757875775262, -143.3755448009918894 ) ) ;
#17405 = CARTESIAN_POINT ( 'NONE',  ( -25.35824191590000254, -1.500000000000000000, -144.8157682190000060 ) ) ;
#17406 = ADVANCED_FACE ( 'NONE', ( #13924 ), #1328, .F. ) ;
#17407 = CARTESIAN_POINT ( 'NONE',  ( -8.514310886093261033, 36.94123471669811209, -140.1199228270031938 ) ) ;
#17408 = ORIENTED_EDGE ( 'NONE', *, *, #16426, .T. ) ;
#17409 = EDGE_CURVE ( 'NONE', #7389, #1186, #15825, .T. ) ;
#17410 = CARTESIAN_POINT ( 'NONE',  ( -20.95225485091065565, 36.93199168240897734, -148.3394883768439456 ) ) ;
#17411 = SURFACE_SIDE_STYLE ('',( #19446 ) ) ;
#17412 = ORIENTED_EDGE ( 'NONE', *, *, #668, .T. ) ;
#17413 = CARTESIAN_POINT ( 'NONE',  ( -6.323999170589999608, 34.61896835509999448, -147.3311432729999808 ) ) ;
#17414 = CARTESIAN_POINT ( 'NONE',  ( 17.33131581010000133, -22.98361965280000163, -146.5552959529999839 ) ) ;
#17415 = CARTESIAN_POINT ( 'NONE',  ( -21.50444101780000139, 40.78041997809999941, -146.2395182369999986 ) ) ;
#17416 = ORIENTED_EDGE ( 'NONE', *, *, #22147, .T. ) ;
#17417 = CARTESIAN_POINT ( 'NONE',  ( 24.38136133040000075, -29.22855050349999928, -146.5552959529999839 ) ) ;
#17418 = DIRECTION ( 'NONE',  ( 4.510774274160000731E-12, -1.321907670990000086E-13, 1.000000000000000000 ) ) ;
#17419 =( GEOMETRIC_REPRESENTATION_CONTEXT ( 3 ) GLOBAL_UNCERTAINTY_ASSIGNED_CONTEXT ( ( #21847 ) ) GLOBAL_UNIT_ASSIGNED_CONTEXT ( ( #15219, #8053, #20804 ) ) REPRESENTATION_CONTEXT ( 'NONE', 'WORKASPACE' ) );
#17420 = ORIENTED_EDGE ( 'NONE', *, *, #23077, .F. ) ;
#17421 = CARTESIAN_POINT ( 'NONE',  ( -31.50000000000000000, -36.00000000000000000, -149.5552959529999839 ) ) ;
#17422 = CARTESIAN_POINT ( 'NONE',  ( -17.62837147338279209, 40.04293477547881963, -142.2225117880255141 ) ) ;
#17423 = DIRECTION ( 'NONE',  ( 0.9957290851625899553, -0.09232328504376198508, -9.001390970786290700E-12 ) ) ;
#17424 = CARTESIAN_POINT ( 'NONE',  ( 7.965536613495201479, 38.40185705422590701, -146.1252975212037484 ) ) ;
#17425 = DIRECTION ( 'NONE',  ( 0.000000000000000000, 0.000000000000000000, 1.000000000000000000 ) ) ;
#17426 = CARTESIAN_POINT ( 'NONE',  ( -25.18528168905853803, 35.37446932239454611, -140.2257898707420054 ) ) ;
#17427 = CARTESIAN_POINT ( 'NONE',  ( 5.809451030008016659, -4.257397883940200245, -150.0552959529999839 ) ) ;
#17428 = CARTESIAN_POINT ( 'NONE',  ( -11.44228618995933111, 41.26819778530094140, -141.7453465123093679 ) ) ;
#17429 = VECTOR ( 'NONE', #5688, 1000.000000000000000 ) ;
#17430 = EDGE_CURVE ( 'NONE', #23438, #328, #1745, .T. ) ;
#17431 = VECTOR ( 'NONE', #17858, 1000.000000000000000 ) ;
#17432 = ORIENTED_EDGE ( 'NONE', *, *, #21896, .F. ) ;
#17433 = FACE_OUTER_BOUND ( 'NONE', #20809, .T. ) ;
#17434 = AXIS2_PLACEMENT_3D ( 'NONE', #21204, #6556, #17503 ) ;
#17435 = ORIENTED_EDGE ( 'NONE', *, *, #22861, .T. ) ;
#17436 = CARTESIAN_POINT ( 'NONE',  ( -34.50000000000000000, -74.00000000000000000, -132.5552959530000123 ) ) ;
#17437 = ORIENTED_EDGE ( 'NONE', *, *, #22602, .T. ) ;
#17438 = AXIS2_PLACEMENT_3D ( 'NONE', #17130, #9506, #22373 ) ;
#17439 = LINE ( 'NONE', #17086, #9444 ) ;
#17440 = ORIENTED_EDGE ( 'NONE', *, *, #1613, .F. ) ;
#17441 = CARTESIAN_POINT ( 'NONE',  ( 4.084326842555937809, 27.61765588495817525, -136.0552959530091641 ) ) ;
#17442 = ORIENTED_EDGE ( 'NONE', *, *, #17807, .F. ) ;
#17443 = ORIENTED_EDGE ( 'NONE', *, *, #19207, .F. ) ;
#17444 = PLANE ( 'NONE',  #2293 ) ;
#17445 = CARTESIAN_POINT ( 'NONE',  ( 32.50000000000000000, 40.03620104890000420, -136.0552959530000123 ) ) ;
#17446 = CARTESIAN_POINT ( 'NONE',  ( 6.499999999879999102, -4.000000000000000000, -135.0552959530000123 ) ) ;
#17447 = CARTESIAN_POINT ( 'NONE',  ( 32.50000000000000000, 39.80430157320000006, -149.8052959529999839 ) ) ;
#17448 = AXIS2_PLACEMENT_3D ( 'NONE', #16870, #22230, #580 ) ;
#17449 = DIRECTION ( 'NONE',  ( 2.257144641399999941E-12, -4.009147065140000298E-51, 1.000000000000000000 ) ) ;
#17450 = ORIENTED_EDGE ( 'NONE', *, *, #6762, .T. ) ;
#17451 = VECTOR ( 'NONE', #5902, 1000.000000000000114 ) ;
#17452 = DIRECTION ( 'NONE',  ( 1.211690350419999855E-27, 2.765629237170000203E-27, -1.000000000000000000 ) ) ;
#17453 = AXIS2_PLACEMENT_3D ( 'NONE', #12674, #14119, #17924 ) ;
#17454 = CARTESIAN_POINT ( 'NONE',  ( -30.99999999989999822, 26.50000000000000000, -139.0552959529999839 ) ) ;
#17455 = VECTOR ( 'NONE', #13774, 1000.000000000000000 ) ;
#17456 = CARTESIAN_POINT ( 'NONE',  ( -32.00000000000000000, -36.00000000000000000, -149.5552959529999839 ) ) ;
#17457 = ORIENTED_EDGE ( 'NONE', *, *, #3451, .F. ) ;
#17458 = EDGE_CURVE ( 'NONE', #10222, #22806, #1218, .T. ) ;
#17459 = DIRECTION ( 'NONE',  ( 0.6459422414661299960, -0.7633862853691516515, 0.000000000000000000 ) ) ;
#17460 = DIRECTION ( 'NONE',  ( 0.000000000000000000, 1.000000000000000000, 0.000000000000000000 ) ) ;
#17461 = VERTEX_POINT ( 'NONE', #21196 ) ;
#17462 = CARTESIAN_POINT ( 'NONE',  ( 1.133692148550000001, 51.50000000000000000, -137.0552959530000123 ) ) ;
#17463 = ADVANCED_FACE ( 'NONE', ( #14042, #19162 ), #22860, .T. ) ;
#17464 = LINE ( 'NONE', #15562, #8180 ) ;
#17465 = VECTOR ( 'NONE', #21631, 1000.000000000000000 ) ;
#17466 = ORIENTED_EDGE ( 'NONE', *, *, #20586, .T. ) ;
#17467 = CARTESIAN_POINT ( 'NONE',  ( -19.59255166829999695, 37.05126161860000167, -140.3061871179999969 ) ) ;
#17468 = CARTESIAN_POINT ( 'NONE',  ( -35.07300000000000040, 16.55147016440000129, -143.5552959529999839 ) ) ;
#17469 = ORIENTED_EDGE ( 'NONE', *, *, #20692, .T. ) ;
#17470 = CARTESIAN_POINT ( 'NONE',  ( -14.68945449529999969, 41.62249060810000145, -143.5408288559999903 ) ) ;
#17471 = CARTESIAN_POINT ( 'NONE',  ( -25.35967232409695526, 32.77444722697165957, -141.6253268585252556 ) ) ;
#17472 = EDGE_LOOP ( 'NONE', ( #11132, #17246, #1979, #3404, #22459, #11179, #11270, #1460, #1549, #20362 ) ) ;
#17473 = CIRCLE ( 'NONE', #10245, 0.7500000000000006661 ) ;
#17474 = VECTOR ( 'NONE', #7519, 1000.000000000000000 ) ;
#17475 = DIRECTION ( 'NONE',  ( 0.000000000000000000, -1.000000000000000000, 0.000000000000000000 ) ) ;
#17476 = ORIENTED_EDGE ( 'NONE', *, *, #1462, .F. ) ;
#17477 = VECTOR ( 'NONE', #9490, 1000.000000000000000 ) ;
#17478 = CARTESIAN_POINT ( 'NONE',  ( -3.500000000000000000, 44.50000000000000000, -150.0552959529999839 ) ) ;
#17479 = CIRCLE ( 'NONE', #12917, 3.500000000000000000 ) ;
#17480 = FACE_OUTER_BOUND ( 'NONE', #13021, .T. ) ;
#17481 = ORIENTED_EDGE ( 'NONE', *, *, #17807, .T. ) ;
#17482 = CARTESIAN_POINT ( 'NONE',  ( 12.50000000020000002, 16.89444872450000190, -136.5552959530000123 ) ) ;
#17483 = CARTESIAN_POINT ( 'NONE',  ( -25.85824191589999899, -34.50000000000000000, -145.5657682190000060 ) ) ;
#17484 = ORIENTED_EDGE ( 'NONE', *, *, #6187, .T. ) ;
#17485 = CYLINDRICAL_SURFACE ( 'NONE', #15921, 1.499999999999999334 ) ;
#17486 = ORIENTED_EDGE ( 'NONE', *, *, #17951, .T. ) ;
#17487 = VECTOR ( 'NONE', #21555, 1000.000000000000000 ) ;
#17488 = COLOUR_RGB ( '', 0.66274510, 0.83137255, 0.94901961) ;
#17489 = LINE ( 'NONE', #10215, #14686 ) ;
#17490 = CARTESIAN_POINT ( 'NONE',  ( 7.683200060759999950, -19.50000000000000000, -143.5552959529999839 ) ) ;
#17491 = CARTESIAN_POINT ( 'NONE',  ( -14.80611810279999929, 41.62812440830000327, -144.5263372940000011 ) ) ;
#17492 = LINE ( 'NONE', #10221, #15569 ) ;
#17493 = VERTEX_POINT ( 'NONE', #17374 ) ;
#17494 = PRESENTATION_STYLE_ASSIGNMENT (( #4651 ) ) ;
#17495 = EDGE_CURVE ( 'NONE', #17118, #6977, #6897, .T. ) ;
#17496 = DIRECTION ( 'NONE',  ( 0.000000000000000000, 1.000000000000000000, 0.000000000000000000 ) ) ;
#17497 = CARTESIAN_POINT ( 'NONE',  ( 20.57808196999505412, -19.71475634692216872, -150.0552959530000123 ) ) ;
#17498 = CARTESIAN_POINT ( 'NONE',  ( 4.499999999879999102, -5.500000000000000000, -135.4552959529999896 ) ) ;
#17499 = CARTESIAN_POINT ( 'NONE',  ( 31.50000000000000000, -39.80430157320000006, -149.5552959529999839 ) ) ;
#17500 = LINE ( 'NONE', #23093, #4137 ) ;
#17501 = ORIENTED_EDGE ( 'NONE', *, *, #20730, .F. ) ;
#17502 = CARTESIAN_POINT ( 'NONE',  ( -16.45586251411692658, 37.06757768449097057, -140.3467090680682929 ) ) ;
#17503 = DIRECTION ( 'NONE',  ( 1.000000000000000000, 0.000000000000000000, -4.510774274160000731E-12 ) ) ;
#17504 = EDGE_CURVE ( 'NONE', #19702, #477, #12357, .T. ) ;
#17505 = DIRECTION ( 'NONE',  ( 2.257083409060000051E-12, 0.000000000000000000, 1.000000000000000000 ) ) ;
#17506 = LINE ( 'NONE', #21207, #9186 ) ;
#17507 = CARTESIAN_POINT ( 'NONE',  ( -7.500000000000000000, 19.50000000000000000, -150.5552959529999839 ) ) ;
#17508 =( GEOMETRIC_REPRESENTATION_CONTEXT ( 3 ) GLOBAL_UNCERTAINTY_ASSIGNED_CONTEXT ( ( #10399 ) ) GLOBAL_UNIT_ASSIGNED_CONTEXT ( ( #6218, #20734, #13832 ) ) REPRESENTATION_CONTEXT ( 'NONE', 'WORKASPACE' ) );
#17509 = ORIENTED_EDGE ( 'NONE', *, *, #22570, .T. ) ;
#17510 = CARTESIAN_POINT ( 'NONE',  ( -10.17933436568690020, 35.38122503049920198, -147.6311798956890016 ) ) ;
#17511 = LINE ( 'NONE', #1234, #2025 ) ;
#17512 = CARTESIAN_POINT ( 'NONE',  ( 3.299140194000170556, -2.580113616947039556, -150.0552959529999839 ) ) ;
#17513 = ORIENTED_EDGE ( 'NONE', *, *, #22575, .T. ) ;
#17514 = PLANE ( 'NONE',  #10661 ) ;
#17515 = EDGE_CURVE ( 'NONE', #1015, #7013, #10449, .T. ) ;
#17516 = CARTESIAN_POINT ( 'NONE',  ( -29.38973091914479951, 34.58161923556721007, -140.8094832672705365 ) ) ;
#17517 = CARTESIAN_POINT ( 'NONE',  ( 15.50000000000000000, 39.50000000000000000, -136.5552959530000123 ) ) ;
#17518 = EDGE_LOOP ( 'NONE', ( #595, #11463, #11892, #16169 ) ) ;
#17519 = CARTESIAN_POINT ( 'NONE',  ( -23.24588518186543951, 41.24341285037552041, -143.7187626422040125 ) ) ;
#17520 = EDGE_CURVE ( 'NONE', #1590, #9187, #19635, .T. ) ;
#17521 = LINE ( 'NONE', #13837, #1013 ) ;
#17522 = ADVANCED_FACE ( 'NONE', ( #14165 ), #8788, .F. ) ;
#17523 = CARTESIAN_POINT ( 'NONE',  ( -6.601136089949999786, -20.10368962670000315, -144.5552959529999839 ) ) ;
#17524 = CARTESIAN_POINT ( 'NONE',  ( 19.00000000000000000, 33.50000000000000000, -136.0552959530000123 ) ) ;
#17525 = ORIENTED_EDGE ( 'NONE', *, *, #11559, .F. ) ;
#17526 = FACE_OUTER_BOUND ( 'NONE', #20584, .T. ) ;
#17527 = AXIS2_PLACEMENT_3D ( 'NONE', #5664, #20199, #18053 ) ;
#17528 = CARTESIAN_POINT ( 'NONE',  ( 22.68320006080000084, -24.50000000000000000, -150.0552959529999839 ) ) ;
#17529 = CIRCLE ( 'NONE', #7272, 6.999999999999999112 ) ;
#17530 = CARTESIAN_POINT ( 'NONE',  ( 9.724682038177496324, -35.50721777958683134, -150.0552959529999839 ) ) ;
#17531 = LINE ( 'NONE', #1251, #9542 ) ;
#17532 = ORIENTED_EDGE ( 'NONE', *, *, #22410, .F. ) ;
#17533 = FILL_AREA_STYLE_COLOUR ( '', #15999 ) ;
#17534 = SURFACE_STYLE_FILL_AREA ( #1133 ) ;
#17535 = EDGE_CURVE ( 'NONE', #14557, #2559, #19620, .T. ) ;
#17536 = ORIENTED_EDGE ( 'NONE', *, *, #11924, .F. ) ;
#17537 = CARTESIAN_POINT ( 'NONE',  ( -7.806459626917139794, 32.86659014882347662, -143.7778124396145927 ) ) ;
#17538 = CARTESIAN_POINT ( 'NONE',  ( -30.02199999990000023, 40.89711431700000333, -146.3052959529999839 ) ) ;
#17539 = DIRECTION ( 'NONE',  ( 0.000000000000000000, -1.000000000000000000, 0.000000000000000000 ) ) ;
#17540 = EDGE_CURVE ( 'NONE', #8058, #213, #6678, .T. ) ;
#17541 = ORIENTED_EDGE ( 'NONE', *, *, #15210, .F. ) ;
#17542 = FACE_OUTER_BOUND ( 'NONE', #23299, .T. ) ;
#17543 = DIRECTION ( 'NONE',  ( -0.9846904924346530086, 0.1743118874569384857, 8.976860394976840322E-12 ) ) ;
#17544 = VECTOR ( 'NONE', #13818, 1000.000000000000000 ) ;
#17545 = CLOSED_SHELL ( 'NONE', ( #10802, #17030, #6026, #8885, #12344, #18661, #7570, #23107, #16945, #19980 ) ) ;
#17546 = ORIENTED_EDGE ( 'NONE', *, *, #17303, .F. ) ;
#17547 = VECTOR ( 'NONE', #6726, 1000.000000000000227 ) ;
#17548 = CYLINDRICAL_SURFACE ( 'NONE', #1564, 1.500000000000001332 ) ;
#17549 = EDGE_CURVE ( 'NONE', #13154, #76, #6660, .T. ) ;
#17550 = CARTESIAN_POINT ( 'NONE',  ( -17.32451618079999633, 37.89224186959999940, -139.5945780149999962 ) ) ;
#17551 = EDGE_CURVE ( 'NONE', #1422, #3284, #16422, .T. ) ;
#17552 = CARTESIAN_POINT ( 'NONE',  ( -16.30969209386606167, -43.75716798044907563, -150.0552959530000123 ) ) ;
#17553 = CARTESIAN_POINT ( 'NONE',  ( 7.759759976971661644, -46.49600213680211169, -136.0552959530175201 ) ) ;
#17554 = EDGE_CURVE ( 'NONE', #4093, #21499, #5228, .T. ) ;
#17555 = CARTESIAN_POINT ( 'NONE',  ( -6.033650297970000409, 36.94170754819999303, -147.9652040070000112 ) ) ;
#17556 = CARTESIAN_POINT ( 'NONE',  ( -24.81824330196665329, 33.37107051305610383, -143.6358663909026916 ) ) ;
#17557 = CARTESIAN_POINT ( 'NONE',  ( 4.301424340775872324, -4.999932770097081480, -150.0552959529999555 ) ) ;
#17558 = DIRECTION ( 'NONE',  ( 0.000000000000000000, 0.000000000000000000, 1.000000000000000000 ) ) ;
#17559 = SHAPE_REPRESENTATION ( 'Spindle Hub', ( #5025 ), #14199 ) ;
#17560 = B_SPLINE_CURVE_WITH_KNOTS ( 'NONE', 3,
 ( #14212, #21718, #8839, #10739, #58, #1731, #12653, #19682, #7066, #3380, #21243, #12182, #17900, #3158, #21596, #1621, #3506, #5280 ),
 .UNSPECIFIED., .F., .F.,
 ( 4, 2, 2, 2, 2, 2, 2, 2, 4 ),
 ( 0.000000000000000000, 0.1250000000000000000, 0.2500000000000000000, 0.3750000000000000000, 0.5000000000000000000, 0.6250000000000000000, 0.7500000000000000000, 0.8750000000000000000, 1.000000000000000000 ),
 .UNSPECIFIED. ) ;
#17561 = EDGE_LOOP ( 'NONE', ( #19340, #11286, #14468, #19820 ) ) ;
#17562 = DIRECTION ( 'NONE',  ( 5.094701932209999624E-24, 1.000000000000000000, -1.149947916579999802E-35 ) ) ;
#17563 = VECTOR ( 'NONE', #3548, 1000.000000000000000 ) ;
#17564 = VECTOR ( 'NONE', #13484, 1000.000000000000000 ) ;
#17565 = UNCERTAINTY_MEASURE_WITH_UNIT (LENGTH_MEASURE( 1.000000000000000082E-05 ), #2121, 'distance_accuracy_value', 'NONE');
#17566 = AXIS2_PLACEMENT_3D ( 'NONE', #4895, #19416, #13698 ) ;
#17567 = EDGE_LOOP ( 'NONE', ( #9726, #505, #17457, #18010 ) ) ;
#17568 = VERTEX_POINT ( 'NONE', #5584 ) ;
#17569 = EDGE_LOOP ( 'NONE', ( #18, #14292, #21783, #5955 ) ) ;
#17570 = CARTESIAN_POINT ( 'NONE',  ( 1.133692148550000001, -50.50000000000000000, -137.0552959530000123 ) ) ;
#17571 = DIRECTION ( 'NONE',  ( -1.000000000000000000, 0.000000000000000000, 0.000000000000000000 ) ) ;
#17572 = ORIENTED_EDGE ( 'NONE', *, *, #10028, .F. ) ;
#17573 = ORIENTED_EDGE ( 'NONE', *, *, #8919, .F. ) ;
#17574 = LINE ( 'NONE', #2817, #7949 ) ;
#17575 = CARTESIAN_POINT ( 'NONE',  ( -9.197324267939999132, 40.96642299180000180, -143.5436038170000188 ) ) ;
#17576 = CARTESIAN_POINT ( 'NONE',  ( -10.98325336546828623, 39.16634992210826738, -141.2646178871198117 ) ) ;
#17577 = CARTESIAN_POINT ( 'NONE',  ( -8.357298602909251528, 35.07902350790208601, -139.9951508849170239 ) ) ;
#17578 = EDGE_CURVE ( 'NONE', #10772, #1657, #1920, .T. ) ;
#17579 = CARTESIAN_POINT ( 'NONE',  ( -9.637198844916387230, 39.82560803348724221, -147.8101000518229853 ) ) ;
#17580 = ORIENTED_EDGE ( 'NONE', *, *, #2686, .T. ) ;
#17581 = CARTESIAN_POINT ( 'NONE',  ( -9.157754307290000284, -15.75963164970000108, -147.5552959529999839 ) ) ;
#17582 = EDGE_CURVE ( 'NONE', #18180, #22397, #1943, .T. ) ;
#17583 = MECHANICAL_DESIGN_GEOMETRIC_PRESENTATION_REPRESENTATION (  '', ( #5419 ), #20253 ) ;
#17584 = AXIS2_PLACEMENT_3D ( 'NONE', #5098, #10550, #17832 ) ;
#17585 = CARTESIAN_POINT ( 'NONE',  ( 5.421820079972371254, -4.699500263597272465, -136.0552959530021155 ) ) ;
#17586 = CARTESIAN_POINT ( 'NONE',  ( -46.50000000000000000, 26.50000000000000000, -148.7506583580000097 ) ) ;
#17587 = ORIENTED_EDGE ( 'NONE', *, *, #10335, .F. ) ;
#17588 = CYLINDRICAL_SURFACE ( 'NONE', #1968, 0.7500000000000013323 ) ;
#17589 = ORIENTED_EDGE ( 'NONE', *, *, #21042, .F. ) ;
#17590 = LINE ( 'NONE', #8524, #6765 ) ;
#17591 = CARTESIAN_POINT ( 'NONE',  ( 18.95053822279999878, 50.00000000000000000, -150.0552959529999839 ) ) ;
#17592 = ORIENTED_EDGE ( 'NONE', *, *, #15465, .F. ) ;
#17593 = CARTESIAN_POINT ( 'NONE',  ( 0.5000000001340000333, 16.89444872450000190, -150.5552959529999839 ) ) ;
#17594 = PLANE ( 'NONE',  #2759 ) ;
#17595 = ORIENTED_EDGE ( 'NONE', *, *, #20846, .T. ) ;
#17596 = CARTESIAN_POINT ( 'NONE',  ( -14.70358821724112630, 36.91864139954906676, -140.0875527721922822 ) ) ;
#17597 = CARTESIAN_POINT ( 'NONE',  ( -4.160432423080000497, -28.71743394529999804, -144.0552959529999839 ) ) ;
#17598 =( GEOMETRIC_REPRESENTATION_CONTEXT ( 3 ) GLOBAL_UNCERTAINTY_ASSIGNED_CONTEXT ( ( #21378 ) ) GLOBAL_UNIT_ASSIGNED_CONTEXT ( ( #13664, #15449, #13796 ) ) REPRESENTATION_CONTEXT ( 'NONE', 'WORKASPACE' ) );
#17599 = ORIENTED_EDGE ( 'NONE', *, *, #8583, .T. ) ;
#17600 = FILL_AREA_STYLE ('',( #19253 ) ) ;
#17601 = EDGE_LOOP ( 'NONE', ( #7169, #4324 ) ) ;
#17602 = CARTESIAN_POINT ( 'NONE',  ( -9.394779979509999990, -17.86685386420000299, -142.5552959529999839 ) ) ;
#17603 = LINE ( 'NONE', #22600, #19862 ) ;
#17604 = ORIENTED_EDGE ( 'NONE', *, *, #3978, .F. ) ;
#17605 = CARTESIAN_POINT ( 'NONE',  ( 1.561837858109999866, -18.84848306830000197, -142.5552959529999839 ) ) ;
#17606 = EDGE_CURVE ( 'NONE', #19847, #2447, #1798, .T. ) ;
#17607 = ADVANCED_FACE ( 'NONE', ( #16532 ), #16304, .F. ) ;
#17608 = LINE ( 'NONE', #6537, #3379 ) ;
#17609 = CARTESIAN_POINT ( 'NONE',  ( -24.16551117139999860, 36.07182940189999698, -148.2420083170000282 ) ) ;
#17610 = EDGE_CURVE ( 'NONE', #9607, #5909, #16185, .T. ) ;
#17611 = ORIENTED_EDGE ( 'NONE', *, *, #4274, .T. ) ;
#17612 = DIRECTION ( 'NONE',  ( -0.9874789572432817186, 0.1577507813030449846, 2.125043109900604696E-14 ) ) ;
#17613 = DIRECTION ( 'NONE',  ( -0.9934078757590584230, 0.1146332952500066366, 4.471042303700267278E-12 ) ) ;
#17614 = CARTESIAN_POINT ( 'NONE',  ( -13.92389048506121441, 38.46313951856771496, -140.8221090936200426 ) ) ;
#17615 = DIRECTION ( 'NONE',  ( -0.6459422414661291079, 0.7633862853691523176, -2.245315045000450442E-12 ) ) ;
#17616 = ORIENTED_EDGE ( 'NONE', *, *, #8288, .T. ) ;
#17617 = FACE_OUTER_BOUND ( 'NONE', #681, .T. ) ;
#17618 = DIRECTION ( 'NONE',  ( 0.1736481776649230202, 0.000000000000000000, -0.9848077530125619594 ) ) ;
#17619 = ADVANCED_FACE ( 'NONE', ( #3574 ), #18205, .T. ) ;
#17620 = DIRECTION ( 'NONE',  ( 1.000000000000000000, 0.000000000000000000, 0.000000000000000000 ) ) ;
#17621 = CARTESIAN_POINT ( 'NONE',  ( -6.024730888589999722, -50.00000000000000000, -151.0552959529999839 ) ) ;
#17622 = CARTESIAN_POINT ( 'NONE',  ( 31.32297112069999656, -40.18599471579999971, -143.0552959529999839 ) ) ;
#17623 = DIRECTION ( 'NONE',  ( 0.000000000000000000, 1.000000000000000000, 0.000000000000000000 ) ) ;
#17624 = EDGE_LOOP ( 'NONE', ( #9990, #16178, #16146, #13490 ) ) ;
#17625 = CYLINDRICAL_SURFACE ( 'NONE', #6888, 10.00000000000000888 ) ;
#17626 = DIRECTION ( 'NONE',  ( 1.000000000000000000, 0.000000000000000000, 0.000000000000000000 ) ) ;
#17627 = FACE_OUTER_BOUND ( 'NONE', #18070, .T. ) ;
#17628 = DIRECTION ( 'NONE',  ( 0.000000000000000000, 1.000000000000000000, 0.000000000000000000 ) ) ;
#17629 = DIRECTION ( 'NONE',  ( 0.000000000000000000, -1.000000000000000000, 2.257144641399999941E-12 ) ) ;
#17630 = ORIENTED_EDGE ( 'NONE', *, *, #6985, .F. ) ;
#17631 = ADVANCED_FACE ( 'NONE', ( #8905 ), #21791, .F. ) ;
#17632 = CYLINDRICAL_SURFACE ( 'NONE', #3913, 6.000000000000002665 ) ;
#17633 = CARTESIAN_POINT ( 'NONE',  ( -32.50000000000000000, -1.000000000000000000, -140.0552959529999839 ) ) ;
#17634 = ADVANCED_FACE ( 'NONE', ( #22010 ), #7479, .F. ) ;
#17635 = EDGE_LOOP ( 'NONE', ( #16460, #1895, #13610, #18696, #124 ) ) ;
#17636 = CARTESIAN_POINT ( 'NONE',  ( -29.45815224830205992, 36.94793816026839295, -140.4653836173367836 ) ) ;
#17637 = DIRECTION ( 'NONE',  ( 1.000000000000000000, 0.000000000000000000, 0.000000000000000000 ) ) ;
#17638 = ORIENTED_EDGE ( 'NONE', *, *, #11081, .F. ) ;
#17639 = CARTESIAN_POINT ( 'NONE',  ( -13.73025257492641060, 37.03482478361183183, -140.6242165752723565 ) ) ;
#17640 = CARTESIAN_POINT ( 'NONE',  ( 6.500000000000000000, 20.50000000000000000, -150.0552959529999839 ) ) ;
#17641 = EDGE_CURVE ( 'NONE', #2758, #14118, #12956, .T. ) ;
#17642 = CARTESIAN_POINT ( 'NONE',  ( -15.50000000000000000, 34.50000000000000000, -137.0552959530000123 ) ) ;
#17643 = CARTESIAN_POINT ( 'NONE',  ( 7.202393543502077833, 37.75405397796894391, -141.6713346540711314 ) ) ;
#17644 = EDGE_LOOP ( 'NONE', ( #15415, #496, #11029, #20885, #101, #10830, #3748 ) ) ;
#17645 = CARTESIAN_POINT ( 'NONE',  ( 4.499999999879999102, -3.500000000000000000, -135.0552959530000123 ) ) ;
#17646 = CARTESIAN_POINT ( 'NONE',  ( 2.742437130618089913, 27.00952979664189968, -150.0552959529999839 ) ) ;
#17647 = CARTESIAN_POINT ( 'NONE',  ( -8.835671558513036317, 38.44113563076084006, -147.4188414315597129 ) ) ;
#17648 = CARTESIAN_POINT ( 'NONE',  ( -9.282104535849999394, -16.71402168319999859, -144.5552959529999839 ) ) ;
#17649 = AXIS2_PLACEMENT_3D ( 'NONE', #20877, #20526, #7775 ) ;
#17650 = ORIENTED_EDGE ( 'NONE', *, *, #15058, .T. ) ;
#17651 =( NAMED_UNIT ( * ) PLANE_ANGLE_UNIT ( ) SI_UNIT ( $, .RADIAN. ) );
#17652 = EDGE_CURVE ( 'NONE', #2146, #5378, #14525, .T. ) ;
#17653 = ORIENTED_EDGE ( 'NONE', *, *, #1906, .F. ) ;
#17654 = CARTESIAN_POINT ( 'NONE',  ( -7.324031428439999658, 35.31041870520000003, -140.2046280479999893 ) ) ;
#17655 = CARTESIAN_POINT ( 'NONE',  ( 25.00000000000000000, -20.50000000000000000, -137.0552959530000123 ) ) ;
#17656 = CARTESIAN_POINT ( 'NONE',  ( -20.65692115970000131, 38.75897267589999728, -140.0270467099999792 ) ) ;
#17657 = EDGE_LOOP ( 'NONE', ( #1254, #2636, #17041, #4052 ) ) ;
#17658 = CARTESIAN_POINT ( 'NONE',  ( -32.50000000000000000, 51.50000000000000000, -151.0552959529999839 ) ) ;
#17659 = CARTESIAN_POINT ( 'NONE',  ( -32.50000000000000000, 14.00000000000000000, -144.0552959529999839 ) ) ;
#17660 = EDGE_CURVE ( 'NONE', #7470, #5559, #9, .T. ) ;
#17661 = ORIENTED_EDGE ( 'NONE', *, *, #1313, .F. ) ;
#17662 = CARTESIAN_POINT ( 'NONE',  ( -21.50145757607925390, 36.99754792876771603, -147.3684231709947312 ) ) ;
#17663 = CARTESIAN_POINT ( 'NONE',  ( 12.91075631260000023, -38.04527125359999928, -147.0552959529999839 ) ) ;
#17664 = DIRECTION ( 'NONE',  ( 1.000000000000000000, 0.000000000000000000, 0.000000000000000000 ) ) ;
#17665 = CARTESIAN_POINT ( 'NONE',  ( 4.800813058695553970, -45.27045733082635337, -136.0552959530108410 ) ) ;
#17666 = DIRECTION ( 'NONE',  ( 4.510774274160000731E-12, -1.321907670990000086E-13, 1.000000000000000000 ) ) ;
#17667 = EDGE_CURVE ( 'NONE', #17230, #19591, #19988, .T. ) ;
#17668 = CARTESIAN_POINT ( 'NONE',  ( 4.750000000030000002, -44.75000000000000000, -137.0552959530000123 ) ) ;
#17669 = DIRECTION ( 'NONE',  ( 0.000000000000000000, 0.000000000000000000, 1.000000000000000000 ) ) ;
#17670 = DIRECTION ( 'NONE',  ( -1.000000000000000000, -2.602084704489999637E-17, 1.701177084830000066E-20 ) ) ;
#17671 = VERTEX_POINT ( 'NONE', #10923 ) ;
#17672 = CARTESIAN_POINT ( 'NONE',  ( -23.51619327739999932, 36.94101002280000046, -140.1031831869999849 ) ) ;
#17673 = ORIENTED_EDGE ( 'NONE', *, *, #11166, .F. ) ;
#17674 = EDGE_CURVE ( 'NONE', #4200, #23177, #17972, .T. ) ;
#17675 = EDGE_CURVE ( 'NONE', #10143, #384, #12605, .T. ) ;
#17676 = ORIENTED_EDGE ( 'NONE', *, *, #3682, .F. ) ;
#17677 = AXIS2_PLACEMENT_3D ( 'NONE', #1504, #12307, #16125 ) ;
#17678 = CARTESIAN_POINT ( 'NONE',  ( 7.085709294149999060, -13.66851965709999916, -142.5552959529999839 ) ) ;
#17679 = DIRECTION ( 'NONE',  ( 0.000000000000000000, 0.000000000000000000, 1.000000000000000000 ) ) ;
#17680 = ORIENTED_EDGE ( 'NONE', *, *, #18855, .T. ) ;
#17681 = EDGE_CURVE ( 'NONE', #1386, #4332, #16640, .T. ) ;
#17682 = VERTEX_POINT ( 'NONE', #9606 ) ;
#17683 = DIRECTION ( 'NONE',  ( 1.526468026909999897E-13, 8.159623473500000156E-13, 1.000000000000000000 ) ) ;
#17684 = EDGE_CURVE ( 'NONE', #1522, #20239, #15220, .T. ) ;
#17685 = CARTESIAN_POINT ( 'NONE',  ( -18.37691940389999701, 35.51168060189999665, -147.4900940509999998 ) ) ;
#17686 = FACE_OUTER_BOUND ( 'NONE', #19851, .T. ) ;
#17687 = CARTESIAN_POINT ( 'NONE',  ( 23.40529971389999986, -31.60139774330000151, -148.5552959529999839 ) ) ;
#17688 = CARTESIAN_POINT ( 'NONE',  ( -7.466450641298933100, 32.18700325849513888, -143.6846124506146509 ) ) ;
#17689 =( REPRESENTATION_RELATIONSHIP ('NONE','NONE', #7672, #3728 ) REPRESENTATION_RELATIONSHIP_WITH_TRANSFORMATION ( #10859 )SHAPE_REPRESENTATION_RELATIONSHIP( ) );
#17690 = VERTEX_POINT ( 'NONE', #22354 ) ;
#17691 = CARTESIAN_POINT ( 'NONE',  ( 8.500000000060001781, 35.50000000000000000, -142.0552959529999839 ) ) ;
#17692 =( BOUNDED_CURVE ( )  B_SPLINE_CURVE ( 5, ( #2678, #4807, #19087, #11931, #15751, #20997, #13850, #15513, #19449, #23013, #9905, #22772 ),
 .UNSPECIFIED., .F., .F. ) 
 B_SPLINE_CURVE_WITH_KNOTS ( ( 6, 3, 3, 6 ),
 ( 0.000000000000000000, 4.469553974960000176, 8.969854531369998440, 13.50363095830000049 ),
 .UNSPECIFIED. ) 
 CURVE ( )  GEOMETRIC_REPRESENTATION_ITEM ( )  RATIONAL_B_SPLINE_CURVE ( ( 0.2500000000000000000, 0.2500000000000000000, 0.2500000000000000000, 0.2500000000000000000, 0.2500000000000000000, 0.2500000000000000000, 0.2500000000000000000, 0.2500000000000000000, 0.2500000000000000000, 0.2500000000000000000, 0.2500000000000000000, 0.2500000000000000000 ) ) 
 REPRESENTATION_ITEM ( '' )  );
#17693 = FACE_OUTER_BOUND ( 'NONE', #211, .T. ) ;
#17694 = VECTOR ( 'NONE', #4189, 1000.000000000000000 ) ;
#17695 = LINE ( 'NONE', #17812, #22787 ) ;
#17696 = VECTOR ( 'NONE', #18977, 1000.000000000000000 ) ;
#17697 = ORIENTED_EDGE ( 'NONE', *, *, #4756, .T. ) ;
#17698 = DIRECTION ( 'NONE',  ( -2.507771768022264771E-12, -1.592655090489709912E-17, 1.000000000000000000 ) ) ;
#17699 = VERTEX_POINT ( 'NONE', #20457 ) ;
#17700 = CARTESIAN_POINT ( 'NONE',  ( 8.500000000060001781, 35.50000000000000000, -146.0552959529999839 ) ) ;
#17701 = CARTESIAN_POINT ( 'NONE',  ( 10.68320006080000084, -21.50000000000000000, -148.5552959529999839 ) ) ;
#17702 = ORIENTED_EDGE ( 'NONE', *, *, #22446, .F. ) ;
#17703 = FACE_OUTER_BOUND ( 'NONE', #9662, .T. ) ;
#17704 = LINE ( 'NONE', #19378, #14530 ) ;
#17705 = ORIENTED_EDGE ( 'NONE', *, *, #3473, .T. ) ;
#17706 = CARTESIAN_POINT ( 'NONE',  ( -21.13851658211848061, 36.11334442976911419, -147.9366295165976055 ) ) ;
#17707 = EDGE_CURVE ( 'NONE', #18121, #3881, #2493, .T. ) ;
#17708 = CARTESIAN_POINT ( 'NONE',  ( -3.499999999959999997, 46.50000000000000000, -136.0552959530000123 ) ) ;
#17709 = ORIENTED_EDGE ( 'NONE', *, *, #8210, .T. ) ;
#17710 = DIRECTION ( 'NONE',  ( 0.000000000000000000, 0.000000000000000000, 1.000000000000000000 ) ) ;
#17711 = ORIENTED_EDGE ( 'NONE', *, *, #4730, .F. ) ;
#17712 = CARTESIAN_POINT ( 'NONE',  ( 16.26251912989999937, -22.62374141290000296, -143.5552959529999839 ) ) ;
#17713 = VECTOR ( 'NONE', #587, 1000.000000000000000 ) ;
#17714 = DIRECTION ( 'NONE',  ( 0.09606172499277226828, 0.9953753789357124848, -8.277822871607614780E-13 ) ) ;
#17715 = ORIENTED_EDGE ( 'NONE', *, *, #17026, .T. ) ;
#17716 = VECTOR ( 'NONE', #10365, 1000.000000000000000 ) ;
#17717 = CARTESIAN_POINT ( 'NONE',  ( 23.00000000000000000, 25.50000000000000000, -150.0552959529999839 ) ) ;
#17718 = CARTESIAN_POINT ( 'NONE',  ( -45.83792946319999828, 29.00000000000000000, -146.9594324700000243 ) ) ;
#17719 = VERTEX_POINT ( 'NONE', #20573 ) ;
#17720 = CARTESIAN_POINT ( 'NONE',  ( -24.06602356359999817, 36.94557182220000158, -148.2530914610000252 ) ) ;
#17721 = VERTEX_POINT ( 'NONE', #4037 ) ;
#17722 = DIRECTION ( 'NONE',  ( 0.000000000000000000, 1.000000000000000000, 0.000000000000000000 ) ) ;
#17723 = FACE_BOUND ( 'NONE', #1633, .T. ) ;
#17724 = CARTESIAN_POINT ( 'NONE',  ( -13.80268676182414112, 38.89075166758362201, -139.8876559908354693 ) ) ;
#17725 = LINE ( 'NONE', #19404, #20894 ) ;
#17726 = VECTOR ( 'NONE', #22033, 1000.000000000000000 ) ;
#17727 = ORIENTED_EDGE ( 'NONE', *, *, #2459, .F. ) ;
#17728 = DIRECTION ( 'NONE',  ( -0.7633862853691524286, 0.6459422414661292189, 1.776356839390353219E-15 ) ) ;
#17729 = LINE ( 'NONE', #15599, #15200 ) ;
#17730 = DIRECTION ( 'NONE',  ( 0.000000000000000000, -1.000000000000000000, 0.000000000000000000 ) ) ;
#17731 = DIRECTION ( 'NONE',  ( 0.000000000000000000, 1.000000000000000000, 0.000000000000000000 ) ) ;
#17732 = EDGE_CURVE ( 'NONE', #17914, #4735, #4151, .T. ) ;
#17733 = DIRECTION ( 'NONE',  ( 2.257749542879999954E-12, 0.000000000000000000, 1.000000000000000000 ) ) ;
#17734 = ORIENTED_EDGE ( 'NONE', *, *, #16598, .T. ) ;
#17735 = DIRECTION ( 'NONE',  ( -1.000000000000000000, 0.000000000000000000, 2.245315044999999693E-12 ) ) ;
#17736 = CARTESIAN_POINT ( 'NONE',  ( -14.60932014329231343, -41.53824377979346139, -136.0552959529670716 ) ) ;
#17737 = DIRECTION ( 'NONE',  ( 0.000000000000000000, 1.000000000000000000, 0.000000000000000000 ) ) ;
#17738 = CARTESIAN_POINT ( 'NONE',  ( -4.855180678435647046, 37.01991258974685906, -139.3889649350431910 ) ) ;
#17739 = CARTESIAN_POINT ( 'NONE',  ( 10.68320006080000084, -20.50000000000000000, -148.5552959529999839 ) ) ;
#17740 = PLANE ( 'NONE',  #8896 ) ;
#17741 = CIRCLE ( 'NONE', #10498, 2.000000000000001776 ) ;
#17742 = EDGE_LOOP ( 'NONE', ( #13096, #15884, #15830, #3983 ) ) ;
#17743 = DIRECTION ( 'NONE',  ( 0.000000000000000000, -1.000000000000000000, 3.568879590630000244E-13 ) ) ;
#17744 = AXIS2_PLACEMENT_3D ( 'NONE', #16298, #1790, #1678 ) ;
#17745 = CARTESIAN_POINT ( 'NONE',  ( -25.07725372939999886, 36.26300138690000097, -147.8685835880000070 ) ) ;
#17746 = ORIENTED_EDGE ( 'NONE', *, *, #7340, .T. ) ;
#17747 = DIRECTION ( 'NONE',  ( 0.000000000000000000, -1.000000000000000000, 0.000000000000000000 ) ) ;
#17748 = DIRECTION ( 'NONE',  ( 0.000000000000000000, 1.000000000000000000, 0.000000000000000000 ) ) ;
#17749 = ORIENTED_EDGE ( 'NONE', *, *, #10598, .F. ) ;
#17750 = LINE ( 'NONE', #8924, #15924 ) ;
#17751 = LINE ( 'NONE', #21453, #13522 ) ;
#17752 = DIRECTION ( 'NONE',  ( 2.257171095940000041E-12, 1.003664318210000046E-28, 1.000000000000000000 ) ) ;
#17753 = CARTESIAN_POINT ( 'NONE',  ( 7.050624870945322087, 36.61023527371315822, -141.5855402290984557 ) ) ;
#17754 = ORIENTED_EDGE ( 'NONE', *, *, #20170, .F. ) ;
#17755 = VECTOR ( 'NONE', #10186, 999.9999999999998863 ) ;
#17756 = LINE ( 'NONE', #15978, #3733 ) ;
#17757 = CARTESIAN_POINT ( 'NONE',  ( 19.00000000000000000, 39.50000000000000000, -150.0552959529999839 ) ) ;
#17758 = ADVANCED_FACE ( 'NONE', ( #22128 ), #4273, .F. ) ;
#17759 = ORIENTED_EDGE ( 'NONE', *, *, #11857, .T. ) ;
#17760 = AXIS2_PLACEMENT_3D ( 'NONE', #9305, #17910, #10745 ) ;
#17761 = ADVANCED_FACE ( 'NONE', ( #8054 ), #11504, .T. ) ;
#17762 = DIRECTION ( 'NONE',  ( 0.9980719161006958995, 0.06206811009758109871, -2.049912714059374948E-13 ) ) ;
#17763 = PRODUCT_CONTEXT ( 'NONE', #2202, 'mechanical' ) ;
#17764 = VECTOR ( 'NONE', #21267, 1000.000000000000000 ) ;
#17765 = EDGE_LOOP ( 'NONE', ( #1472, #5221, #11226, #23472 ) ) ;
#17766 = CARTESIAN_POINT ( 'NONE',  ( -7.220568065030000149, 34.52259161599999970, -140.6708207100000152 ) ) ;
#17767 = DIRECTION ( 'NONE',  ( 0.6459422414661291079, -0.7633862853691523176, 2.245315045000450442E-12 ) ) ;
#17768 = DIRECTION ( 'NONE',  ( 0.000000000000000000, 1.000000000000000000, 0.000000000000000000 ) ) ;
#17769 = VERTEX_POINT ( 'NONE', #11389 ) ;
#17770 = CARTESIAN_POINT ( 'NONE',  ( -4.740745377981987474, 37.03357229753903113, -140.5852769424096493 ) ) ;
#17771 = CARTESIAN_POINT ( 'NONE',  ( 12.50000000010000001, 24.10555127549999810, -143.5552959529999839 ) ) ;
#17772 = ORIENTED_EDGE ( 'NONE', *, *, #19703, .T. ) ;
#17773 = LINE ( 'NONE', #23257, #21707 ) ;
#17774 = DIRECTION ( 'NONE',  ( 1.526468026909999897E-13, 8.159623473500000156E-13, 1.000000000000000000 ) ) ;
#17775 = AXIS2_PLACEMENT_3D ( 'NONE', #9713, #7373, #16639 ) ;
#17776 = LINE ( 'NONE', #11940, #5566 ) ;
#17777 = VECTOR ( 'NONE', #12320, 1000.000000000000000 ) ;
#17778 = CARTESIAN_POINT ( 'NONE',  ( 8.698929461760148030, -45.27072668386799137, -136.0552959530196233 ) ) ;
#17779 = EDGE_CURVE ( 'NONE', #16387, #3836, #9714, .T. ) ;
#17780 = CARTESIAN_POINT ( 'NONE',  ( -19.86630785140000199, -51.50000000000000000, -137.0552959530000123 ) ) ;
#17781 = DIRECTION ( 'NONE',  ( -8.523837997462170112E-12, 0.000000000000000000, 1.000000000000000000 ) ) ;
#17782 = APPLICATION_PROTOCOL_DEFINITION ( 'draft international standard', 'automotive_design', 1998, #5834 ) ;
#17783 = DIRECTION ( 'NONE',  ( 2.257157423930000049E-12, 0.000000000000000000, 1.000000000000000000 ) ) ;
#17784 = CARTESIAN_POINT ( 'NONE',  ( -3.499999999959999997, 42.50000000000000000, -136.0552959530000123 ) ) ;
#17785 = EDGE_LOOP ( 'NONE', ( #8359, #10400, #20322, #16806 ) ) ;
#17786 = CARTESIAN_POINT ( 'NONE',  ( -23.64946213540040887, 37.84712475405090260, -139.7583381698287042 ) ) ;
#17787 = EDGE_CURVE ( 'NONE', #3534, #21497, #4380, .T. ) ;
#17788 = UNCERTAINTY_MEASURE_WITH_UNIT (LENGTH_MEASURE( 1.000000000000000082E-05 ), #10018, 'distance_accuracy_value', 'NONE');
#17790 = ORIENTED_EDGE ( 'NONE', *, *, #21919, .F. ) ;
#17789 = VECTOR ( 'NONE', #14590, 1000.000000000000227 ) ;
#17791 = VECTOR ( 'NONE', #798, 1000.000000000000000 ) ;
#17792 = ORIENTED_EDGE ( 'NONE', *, *, #18782, .F. ) ;
#17793 = CARTESIAN_POINT ( 'NONE',  ( -15.46613156818549939, 36.99333119717887541, -147.5584717933951708 ) ) ;
#17794 = CARTESIAN_POINT ( 'NONE',  ( -28.33971964074914851, 37.08144121879573163, -140.0461821376498506 ) ) ;
#17795 = CARTESIAN_POINT ( 'NONE',  ( 25.00000000000000000, -20.50000000000000000, -137.2152959530000089 ) ) ;
#17796 = ORIENTED_EDGE ( 'NONE', *, *, #14309, .T. ) ;
#17797 = DIRECTION ( 'NONE',  ( -2.257144641399999941E-12, 8.049635416090000264E-35, -1.000000000000000000 ) ) ;
#17798 = EDGE_CURVE ( 'NONE', #13760, #15090, #704, .T. ) ;
#17799 = CARTESIAN_POINT ( 'NONE',  ( -15.36599175859999988, 37.73046438850000328, -147.5598381920000008 ) ) ;
#17800 = CARTESIAN_POINT ( 'NONE',  ( 8.900000000049999471, 39.46779253580000102, -149.5552959529999839 ) ) ;
#17801 = LINE ( 'NONE', #21624, #17764 ) ;
#17802 = ORIENTED_EDGE ( 'NONE', *, *, #17675, .F. ) ;
#17803 = PLANE ( 'NONE',  #6487 ) ;
#17804 = ORIENTED_EDGE ( 'NONE', *, *, #8331, .T. ) ;
#17805 = CARTESIAN_POINT ( 'NONE',  ( 9.551261401524259398, 35.93001144567825378, -141.7958383017457038 ) ) ;
#17806 = VECTOR ( 'NONE', #7549, 1000.000000000000227 ) ;
#17807 = EDGE_CURVE ( 'NONE', #15585, #2014, #5928, .T. ) ;
#17808 = VECTOR ( 'NONE', #16976, 1000.000000000000000 ) ;
#17809 = PLANE ( 'NONE',  #16329 ) ;
#17810 = ADVANCED_FACE ( 'NONE', ( #20805 ), #2262, .F. ) ;
#17811 = AXIS2_PLACEMENT_3D ( 'NONE', #23032, #17562, #12752 ) ;
#17812 = CARTESIAN_POINT ( 'NONE',  ( -38.39535039420000118, 47.50000000000000000, -147.5552959529999839 ) ) ;
#17813 = VERTEX_POINT ( 'NONE', #18893 ) ;
#17814 = VECTOR ( 'NONE', #21721, 1000.000000000000000 ) ;
#17815 = ADVANCED_FACE ( 'NONE', ( #352 ), #2384, .T. ) ;
#17816 = VECTOR ( 'NONE', #21300, 1000.000000000000000 ) ;
#17817 = ADVANCED_FACE ( 'NONE', ( #13184 ), #13532, .T. ) ;
#17818 = CARTESIAN_POINT ( 'NONE',  ( 8.750000000030000891, -2.273736754430000208E-12, -136.0552959530000123 ) ) ;
#17819 = ORIENTED_EDGE ( 'NONE', *, *, #15587, .F. ) ;
#17820 = DIRECTION ( 'NONE',  ( 0.000000000000000000, 2.257144641399999941E-12, -1.000000000000000000 ) ) ;
#17821 = DIRECTION ( 'NONE',  ( 0.000000000000000000, 0.000000000000000000, 1.000000000000000000 ) ) ;
#17822 = ORIENTED_EDGE ( 'NONE', *, *, #10074, .T. ) ;
#17823 = CARTESIAN_POINT ( 'NONE',  ( 26.50000000000000711, -20.89269908169871570, -150.0552959529999839 ) ) ;
#17824 = EDGE_LOOP ( 'NONE', ( #1414, #13659, #14232, #6915 ) ) ;
#17825 = CARTESIAN_POINT ( 'NONE',  ( -22.21135766849999982, 35.30661492690000358, -147.9492090369999744 ) ) ;
#17826 = CARTESIAN_POINT ( 'NONE',  ( -5.101575545681980017, 43.27312978694517653, -150.0552959529999839 ) ) ;
#17827 = VERTEX_POINT ( 'NONE', #13072 ) ;
#17828 = AXIS2_PLACEMENT_3D ( 'NONE', #13062, #9704, #7585 ) ;
#17829 = VERTEX_POINT ( 'NONE', #4496 ) ;
#17830 = CARTESIAN_POINT ( 'NONE',  ( -26.49522641139999735, 37.71913029610000478, -140.3749603070000092 ) ) ;
#17831 = VECTOR ( 'NONE', #6020, 1000.000000000000000 ) ;
#17832 = DIRECTION ( 'NONE',  ( 1.000000000000000000, 0.000000000000000000, 0.000000000000000000 ) ) ;
#17833 = EDGE_LOOP ( 'NONE', ( #7429, #3673, #23224, #19379 ) ) ;
#17834 = FACE_OUTER_BOUND ( 'NONE', #10596, .T. ) ;
#17835 =( BOUNDED_SURFACE ( )  B_SPLINE_SURFACE ( 5, 5, ( 
 ( #13443, #4404, #11645, #18922, #2634, #858 ),
 ( #15820, #19274, #12473, #16062, #14038, #13811 ),
 ( #21075, #17724, #21193, #22971, #17614, #10687 ),
 ( #23204, #23086, #12124, #1567, #1325, #5000 ),
 ( #12243, #19757, #23320, #8784, #21308, #10562 ),
 ( #3453, #6893, #17968, #2983, #1680, #6543 ),
 ( #17491, #15594, #3215, #10446, #22856, #7011 ),
 ( #1440, #4761, #12009, #19403, #12354, #14274 ),
 ( #14161, #8659, #3103, #21542, #10220, #1215 ),
 ( #8441, #5224, #21425, #15942, #3326, #15709 ),
 ( #17848, #6656, #13919, #4877, #19630, #10339 ),
 ( #8546, #5110, #6773, #19521, #1916, #10797 ) ),
 .UNSPECIFIED., .F., .F., .F. ) 
 B_SPLINE_SURFACE_WITH_KNOTS ( ( 6, 3, 3, 6 ),
 ( 6, 6 ),
 ( 0.000000000000000000, 4.151671928079999851, 8.316542232069998875, 12.50501063799999990 ),
 ( 0.000000000000000000, 1.570796326821630062 ),
 .UNSPECIFIED. ) 
 GEOMETRIC_REPRESENTATION_ITEM ( )  RATIONAL_B_SPLINE_SURFACE ( (
 ( 1.000000000000000000, 0.5999999999932189576, 0.3999999999932190020, 0.2999999999949140017, 0.2499999999966094899, 0.2500000000000000000),
 ( 1.000000000000000000, 0.5999999999932189576, 0.3999999999932190020, 0.2999999999949140017, 0.2499999999966094899, 0.2500000000000000000),
 ( 1.000000000000000000, 0.5999999999932189576, 0.3999999999932190020, 0.2999999999949140017, 0.2499999999966094899, 0.2500000000000000000),
 ( 1.000000000000000000, 0.5999999999932189576, 0.3999999999932190020, 0.2999999999949140017, 0.2499999999966094899, 0.2500000000000000000),
 ( 1.000000000000000000, 0.5999999999932189576, 0.3999999999932190020, 0.2999999999949140017, 0.2499999999966094899, 0.2500000000000000000),
 ( 1.000000000000000000, 0.5999999999932189576, 0.3999999999932190020, 0.2999999999949140017, 0.2499999999966094899, 0.2500000000000000000),
 ( 1.000000000000000000, 0.5999999999932189576, 0.3999999999932190020, 0.2999999999949140017, 0.2499999999966094899, 0.2500000000000000000),
 ( 1.000000000000000000, 0.5999999999932189576, 0.3999999999932190020, 0.2999999999949140017, 0.2499999999966094899, 0.2500000000000000000),
 ( 1.000000000000000000, 0.5999999999932189576, 0.3999999999932190020, 0.2999999999949140017, 0.2499999999966094899, 0.2500000000000000000),
 ( 1.000000000000000000, 0.5999999999932189576, 0.3999999999932190020, 0.2999999999949140017, 0.2499999999966094899, 0.2500000000000000000),
 ( 1.000000000000000000, 0.5999999999932189576, 0.3999999999932190020, 0.2999999999949140017, 0.2499999999966094899, 0.2500000000000000000),
 ( 1.000000000000000000, 0.5999999999932189576, 0.3999999999932190020, 0.2999999999949140017, 0.2499999999966094899, 0.2500000000000000000) ) ) 
 REPRESENTATION_ITEM ( '' )  SURFACE ( )  );
#17836 = AXIS2_PLACEMENT_3D ( 'NONE', #7489, #14754, #22021 ) ;
#17837 = AXIS2_PLACEMENT_3D ( 'NONE', #16937, #7657, #773 ) ;
#17838 = DIRECTION ( 'NONE',  ( 4.510774274160000731E-12, -1.321907670990000086E-13, 1.000000000000000000 ) ) ;
#17839 = EDGE_LOOP ( 'NONE', ( #1961, #13627, #13325, #4758 ) ) ;
#17840 = CARTESIAN_POINT ( 'NONE',  ( -15.67014142459999881, 35.45905754580000036, -147.3461856840000053 ) ) ;
#17841 = EDGE_CURVE ( 'NONE', #1248, #14370, #21671, .T. ) ;
#17842 = EDGE_CURVE ( 'NONE', #2559, #7276, #15911, .T. ) ;
#17843 = ORIENTED_EDGE ( 'NONE', *, *, #8509, .T. ) ;
#17844 = DIRECTION ( 'NONE',  ( 2.507771768020000122E-12, -0.000000000000000000, -1.000000000000000000 ) ) ;
#17845 = AXIS2_PLACEMENT_3D ( 'NONE', #7035, #21569, #3349 ) ;
#17846 = CARTESIAN_POINT ( 'NONE',  ( -20.96728015145808044, -4.669278027980419132, -146.3157682190065145 ) ) ;
#17847 = VECTOR ( 'NONE', #23436, 1000.000000000000000 ) ;
#17848 = CARTESIAN_POINT ( 'NONE',  ( -15.47708384459999920, 37.95279615419999431, -148.5507537150000132 ) ) ;
#17849 = DIRECTION ( 'NONE',  ( 0.7071067811865475727, 0.7071067811865475727, 0.000000000000000000 ) ) ;
#17850 = ORIENTED_EDGE ( 'NONE', *, *, #17328, .T. ) ;
#17851 = CARTESIAN_POINT ( 'NONE',  ( -3.499999999959999997, 34.00000000000000000, -153.0552959529999839 ) ) ;
#17852 = VECTOR ( 'NONE', #16972, 1000.000000000000000 ) ;
#17853 = VECTOR ( 'NONE', #1392, 1000.000000000000000 ) ;
#17854 = FACE_BOUND ( 'NONE', #13130, .T. ) ;
#17855 = PLANE ( 'NONE',  #13668 ) ;
#17856 = LINE ( 'NONE', #5231, #5009 ) ;
#17857 = VECTOR ( 'NONE', #6832, 1000.000000000000000 ) ;
#17858 = DIRECTION ( 'NONE',  ( -1.000000000000000000, 0.000000000000000000, 0.000000000000000000 ) ) ;
#17859 = AXIS2_PLACEMENT_3D ( 'NONE', #11519, #369, #7608 ) ;
#17860 = VERTEX_POINT ( 'NONE', #17701 ) ;
#17861 = CARTESIAN_POINT ( 'NONE',  ( 0.1832000607640000001, -3.000000000000000000, -150.0552959529999839 ) ) ;
#17862 = CARTESIAN_POINT ( 'NONE',  ( -15.00000000000000000, -41.50000000000000000, -136.0552959530000123 ) ) ;
#17863 = DIRECTION ( 'NONE',  ( -1.000000000000000000, 0.000000000000000000, 0.000000000000000000 ) ) ;
#17864 = CARTESIAN_POINT ( 'NONE',  ( -5.241146848258035007, 41.27390541520301781, -144.5340427261826051 ) ) ;
#17865 = CARTESIAN_POINT ( 'NONE',  ( -8.514310886080000529, 36.94123471670000214, -140.1199228270000106 ) ) ;
#17866 = CARTESIAN_POINT ( 'NONE',  ( -15.00000000000000000, -44.50000000000000000, -136.0552959530000123 ) ) ;
#17867 = ORIENTED_EDGE ( 'NONE', *, *, #21807, .F. ) ;
#17868 = CARTESIAN_POINT ( 'NONE',  ( -26.49522641139999735, 37.71913029610000478, -140.3749603070000092 ) ) ;
#17869 = CARTESIAN_POINT ( 'NONE',  ( -15.57786843150000067, 37.00666880280000726, -148.5521201120000114 ) ) ;
#17870 = VERTEX_POINT ( 'NONE', #4974 ) ;
#17871 = VECTOR ( 'NONE', #8271, 1000.000000000000000 ) ;
#17872 = AXIS2_PLACEMENT_3D ( 'NONE', #7059, #16348, #53 ) ;
#17873 = EDGE_CURVE ( 'NONE', #232, #12791, #17464, .T. ) ;
#17874 = VECTOR ( 'NONE', #2318, 1000.000000000000114 ) ;
#17875 = ADVANCED_FACE ( 'NONE', ( #1411 ), #3191, .T. ) ;
#17876 = CARTESIAN_POINT ( 'NONE',  ( 25.00000000000000000, -20.50000000000000000, -135.0552959530000123 ) ) ;
#17877 = VERTEX_POINT ( 'NONE', #15688 ) ;
#17878 = CARTESIAN_POINT ( 'NONE',  ( -24.10813950015861451, 36.95059904175489862, -147.5089432697649556 ) ) ;
#17879 = CARTESIAN_POINT ( 'NONE',  ( 12.91075631260000023, -38.04527125359999928, -146.5552959529999839 ) ) ;
#17880 = DIRECTION ( 'NONE',  ( 1.000000000000000000, 0.000000000000000000, 0.000000000000000000 ) ) ;
#17881 = CARTESIAN_POINT ( 'NONE',  ( 7.127308729211550009, 37.60485668770037648, -141.6295540220406508 ) ) ;
#17882 = ORIENTED_EDGE ( 'NONE', *, *, #13893, .T. ) ;
#17883 = CARTESIAN_POINT ( 'NONE',  ( 8.750000000030000891, -36.98606797749999942, -137.0552959530000123 ) ) ;
#17884 = CARTESIAN_POINT ( 'NONE',  ( 16.29836742280000195, -22.74229684829999698, -143.5552959529999839 ) ) ;
#17885 = CARTESIAN_POINT ( 'NONE',  ( -8.869124888310000898, 38.72872035620000020, -148.0517159070000162 ) ) ;
#17886 = CARTESIAN_POINT ( 'NONE',  ( -15.61190926919999988, -18.00000000000000000, -146.8816477750000047 ) ) ;
#17887 = ORIENTED_EDGE ( 'NONE', *, *, #22496, .F. ) ;
#17888 = VECTOR ( 'NONE', #12488, 1000.000000000000000 ) ;
#17889 = CARTESIAN_POINT ( 'NONE',  ( 19.71905350744767205, 19.57650987476679916, -136.0552959530445492 ) ) ;
#17890 = VERTEX_POINT ( 'NONE', #12098 ) ;
#17891 = FACE_OUTER_BOUND ( 'NONE', #1464, .T. ) ;
#17892 = DIRECTION ( 'NONE',  ( 1.000000000000000000, 0.000000000000000000, -1.526556658859589738E-13 ) ) ;
#17893 = DIRECTION ( 'NONE',  ( -4.510774274160000731E-12, 1.321907670990000086E-13, -1.000000000000000000 ) ) ;
#17894 = ORIENTED_EDGE ( 'NONE', *, *, #4950, .F. ) ;
#17895 = CARTESIAN_POINT ( 'NONE',  ( -5.647208160094595364, 36.92537127315257806, -140.1716802708971557 ) ) ;
#17896 = CARTESIAN_POINT ( 'NONE',  ( -32.50000000000000000, 21.50000000000000000, -151.0552959529999839 ) ) ;
#17897 = ORIENTED_EDGE ( 'NONE', *, *, #16490, .T. ) ;
#17898 = CYLINDRICAL_SURFACE ( 'NONE', #15982, 1.500000000000001998 ) ;
#17899 = ADVANCED_FACE ( 'NONE', ( #19375 ), #6394, .F. ) ;
#17900 = CARTESIAN_POINT ( 'NONE',  ( 18.09818317339652083, 24.33939095839998856, -150.0552959529999839 ) ) ;
#17901 = CARTESIAN_POINT ( 'NONE',  ( -35.73252798949999942, 47.50000000000000000, -140.5552959529999839 ) ) ;
#17902 = VECTOR ( 'NONE', #19946, 1000.000000000000000 ) ;
#17903 = EDGE_CURVE ( 'NONE', #7233, #9003, #8167, .T. ) ;
#17904 = VECTOR ( 'NONE', #2008, 1000.000000000000000 ) ;
#17905 = CARTESIAN_POINT ( 'NONE',  ( 5.740346993259798580, -46.49619218629824502, -136.0552959530129726 ) ) ;
#17906 = VECTOR ( 'NONE', #9296, 1000.000000000000000 ) ;
#17907 = FACE_OUTER_BOUND ( 'NONE', #20539, .T. ) ;
#17908 = CARTESIAN_POINT ( 'NONE',  ( 12.91075631260000023, -38.04527125359999928, -146.5552959529999839 ) ) ;
#17909 = APPLICATION_PROTOCOL_DEFINITION ( 'draft international standard', 'automotive_design', 1998, #19210 ) ;
#17910 = DIRECTION ( 'NONE',  ( 3.994014902950000436E-29, -1.000000000000000000, 4.148443855749999753E-27 ) ) ;
#17911 = CARTESIAN_POINT ( 'NONE',  ( -35.47299999999999898, 16.95803989150000035, -144.5552959529999839 ) ) ;
#17912 = B_SPLINE_CURVE_WITH_KNOTS ( 'NONE', 1,
 ( #10223, #6659 ),
 .UNSPECIFIED., .F., .F.,
 ( 2, 2 ),
 ( -6.000000000000000000, 6.000000000000000000 ),
 .UNSPECIFIED. ) ;
#17913 = CARTESIAN_POINT ( 'NONE',  ( -15.50000000000000000, 47.50000000000000000, -151.0552959529999839 ) ) ;
#17914 = VERTEX_POINT ( 'NONE', #17591 ) ;
#17915 = ORIENTED_EDGE ( 'NONE', *, *, #2994, .T. ) ;
#17916 = ORIENTED_EDGE ( 'NONE', *, *, #1006, .F. ) ;
#17917 = DIRECTION ( 'NONE',  ( 5.094701932209999624E-24, 1.000000000000000000, 0.000000000000000000 ) ) ;
#17918 = CARTESIAN_POINT ( 'NONE',  ( -28.59946202397140169, 34.31616424879415916, -140.2812573677312002 ) ) ;
#17919 = ORIENTED_EDGE ( 'NONE', *, *, #23077, .T. ) ;
#17920 = VECTOR ( 'NONE', #4656, 1000.000000000000000 ) ;
#17921 = CARTESIAN_POINT ( 'NONE',  ( 3.611688725869999975E-11, 39.50000000000000000, -136.0552959530000123 ) ) ;
#17922 = VECTOR ( 'NONE', #19055, 1000.000000000000000 ) ;
#17923 = ORIENTED_EDGE ( 'NONE', *, *, #1084, .F. ) ;
#17924 = DIRECTION ( 'NONE',  ( 1.000000000000000000, 0.000000000000000000, -4.429789868254374596E-12 ) ) ;
#17925 = CARTESIAN_POINT ( 'NONE',  ( -19.79184979336553241, 37.02747215728108188, -140.6521846888477114 ) ) ;
#17926 = CARTESIAN_POINT ( 'NONE',  ( -11.66591920674827065, 38.51472844954471242, -147.7933753654626798 ) ) ;
#17927 = CARTESIAN_POINT ( 'NONE',  ( -7.499999999969999109, 19.50000000000000000, -136.5552959530000123 ) ) ;
#17928 = ORIENTED_EDGE ( 'NONE', *, *, #6327, .T. ) ;
#17929 = FACE_OUTER_BOUND ( 'NONE', #14063, .T. ) ;
#17930 = ORIENTED_EDGE ( 'NONE', *, *, #19734, .F. ) ;
#17931 = DIRECTION ( 'NONE',  ( 1.000000000000000000, 0.000000000000000000, 0.000000000000000000 ) ) ;
#17932 = EDGE_CURVE ( 'NONE', #17877, #3870, #22950, .T. ) ;
#17933 = CARTESIAN_POINT ( 'NONE',  ( 8.250000000000000000, -40.23606797749999942, -150.0552959529999839 ) ) ;
#17934 = CARTESIAN_POINT ( 'NONE',  ( -32.50000000000000000, -51.50000000000000000, -142.8052959529999839 ) ) ;
#17935 = VECTOR ( 'NONE', #22476, 1000.000000000000000 ) ;
#17936 = ORIENTED_EDGE ( 'NONE', *, *, #6298, .F. ) ;
#17937 = VECTOR ( 'NONE', #22516, 1000.000000000000000 ) ;
#17938 = VECTOR ( 'NONE', #16456, 1000.000000000000227 ) ;
#17939 = ADVANCED_FACE ( 'NONE', ( #15439 ), #6633, .T. ) ;
#17940 = CARTESIAN_POINT ( 'NONE',  ( 27.68320006080000084, -34.50000000000000000, -149.3052959529999839 ) ) ;
#17941 = ORIENTED_EDGE ( 'NONE', *, *, #3364, .F. ) ;
#17942 = DIRECTION ( 'NONE',  ( 2.257171095940000041E-12, 1.003664318210000046E-28, 1.000000000000000000 ) ) ;
#17943 = PLANE ( 'NONE',  #4425 ) ;
#17944 = ORIENTED_EDGE ( 'NONE', *, *, #18279, .F. ) ;
#17945 = CARTESIAN_POINT ( 'NONE',  ( -32.50000000000000000, 46.00000000000000000, -146.5552959529999839 ) ) ;
#17946 = ORIENTED_EDGE ( 'NONE', *, *, #9808, .T. ) ;
#17947 = DIRECTION ( 'NONE',  ( 4.430318231639999944E-12, -6.100259101500000139E-13, 1.000000000000000000 ) ) ;
#17948 = PLANE ( 'NONE',  #7966 ) ;
#17949 = ORIENTED_EDGE ( 'NONE', *, *, #15210, .T. ) ;
#17950 = DIRECTION ( 'NONE',  ( 0.000000000000000000, 0.000000000000000000, 1.000000000000000000 ) ) ;
#17951 = EDGE_CURVE ( 'NONE', #7723, #14599, #7442, .T. ) ;
#17952 = EDGE_LOOP ( 'NONE', ( #3525, #10320, #3398, #7147 ) ) ;
#17953 = CARTESIAN_POINT ( 'NONE',  ( -26.39256767694444150, 41.50003988677031685, -143.5805134116744171 ) ) ;
#17954 = DIRECTION ( 'NONE',  ( -0.9913873220698726785, 0.1309625047069831461, -1.853446743629759619E-14 ) ) ;
#17955 = ORIENTED_EDGE ( 'NONE', *, *, #19756, .T. ) ;
#17956 =( GEOMETRIC_REPRESENTATION_CONTEXT ( 3 ) GLOBAL_UNCERTAINTY_ASSIGNED_CONTEXT ( ( #11104 ) ) GLOBAL_UNIT_ASSIGNED_CONTEXT ( ( #23502, #72, #5872 ) ) REPRESENTATION_CONTEXT ( 'NONE', 'WORKASPACE' ) );
#17957 = CARTESIAN_POINT ( 'NONE',  ( 0.1832000607640000001, -3.000000000000000000, -148.5552959529999839 ) ) ;
#17958 = AXIS2_PLACEMENT_3D ( 'NONE', #20356, #7954, #22022 ) ;
#17959 = CARTESIAN_POINT ( 'NONE',  ( -11.11377970773875923, 36.98904460433606545, -140.6889018750556772 ) ) ;
#17960 = CARTESIAN_POINT ( 'NONE',  ( 24.97526911139999939, -44.90215078659999648, -151.0552959529999839 ) ) ;
#17961 = VERTEX_POINT ( 'NONE', #21281 ) ;
#17962 = CARTESIAN_POINT ( 'NONE',  ( 6.000000000000000000, -3.500000000000000000, -145.5552959529999839 ) ) ;
#17963 = EDGE_CURVE ( 'NONE', #13650, #19480, #15798, .T. ) ;
#17964 = VERTEX_POINT ( 'NONE', #8636 ) ;
#17965 = DIRECTION ( 'NONE',  ( 0.000000000000000000, 1.000000000000000000, 0.000000000000000000 ) ) ;
#17966 = CARTESIAN_POINT ( 'NONE',  ( -11.59475511489694988, 36.93163239416678323, -139.6817994052732388 ) ) ;
#17967 = ADVANCED_FACE ( 'NONE', ( #2729 ), #6747, .T. ) ;
#17968 = CARTESIAN_POINT ( 'NONE',  ( -14.08453874197354416, 41.33416090294871026, -143.6415802795030743 ) ) ;
#17969 = CARTESIAN_POINT ( 'NONE',  ( -28.47499893025420548, 37.06529344306947138, -140.4421442387196350 ) ) ;
#17970 = EDGE_LOOP ( 'NONE', ( #6415, #16587, #16950, #16095, #11138, #14708, #13632, #2651, #15564, #10719, #18353, #8035, #21261, #8084, #3566 ) ) ;
#17971 = DIRECTION ( 'NONE',  ( -1.000000000000000000, -5.988019148734350335E-18, 1.096099552913726042E-17 ) ) ;
#17972 = LINE ( 'NONE', #18086, #16190 ) ;
#17973 = EDGE_CURVE ( 'NONE', #22352, #22041, #20929, .T. ) ;
#17974 = AXIS2_PLACEMENT_3D ( 'NONE', #9538, #13576, #4077 ) ;
#17975 = FACE_OUTER_BOUND ( 'NONE', #3169, .T. ) ;
#17976 = DIRECTION ( 'NONE',  ( 0.9985681355238719137, -0.05349466063429310358, -4.512926597569420539E-12 ) ) ;
#17977 = DIRECTION ( 'NONE',  ( 0.000000000000000000, -1.000000000000000000, 0.000000000000000000 ) ) ;
#17978 = CARTESIAN_POINT ( 'NONE',  ( 1.352544480119999948, -20.86379603889999856, -145.5552959529999839 ) ) ;
#17979 = ORIENTED_EDGE ( 'NONE', *, *, #18385, .F. ) ;
#17980 = LINE ( 'NONE', #1691, #5750 ) ;
#17981 = EDGE_CURVE ( 'NONE', #9331, #12346, #13786, .T. ) ;
#17982 = DIRECTION ( 'NONE',  ( 2.257157423930000049E-12, 0.000000000000000000, 1.000000000000000000 ) ) ;
#17983 = DIRECTION ( 'NONE',  ( 2.257144641399999941E-12, -4.009147065140000298E-51, 1.000000000000000000 ) ) ;
#17984 = ADVANCED_FACE ( 'NONE', ( #940 ), #19134, .T. ) ;
#17985 = CARTESIAN_POINT ( 'NONE',  ( -6.044964120310517330, 41.66664426582369174, -143.4739125349191795 ) ) ;
#17986 = LINE ( 'NONE', #8916, #15953 ) ;
#17987 = ADVANCED_FACE ( 'NONE', ( #6519, #4736 ), #11980, .F. ) ;
#17988 = VERTEX_POINT ( 'NONE', #8418 ) ;
#17989 = CARTESIAN_POINT ( 'NONE',  ( 10.17780667183982501, -21.37282441786776488, -148.5552959529999555 ) ) ;
#17990 = ADVANCED_FACE ( 'NONE', ( #19848 ), #3424, .F. ) ;
#17991 = FACE_BOUND ( 'NONE', #1638, .T. ) ;
#17992 = AXIS2_PLACEMENT_3D ( 'NONE', #3668, #17710, #12580 ) ;
#17993 = ORIENTED_EDGE ( 'NONE', *, *, #19396, .F. ) ;
#17994 = CARTESIAN_POINT ( 'NONE',  ( -3.500000000000000000, 46.50000000000000000, -150.0552959529999839 ) ) ;
#17995 = VERTEX_POINT ( 'NONE', #3777 ) ;
#17996 = CARTESIAN_POINT ( 'NONE',  ( -24.74875653007431708, 37.76084906505778349, -147.5435553219018061 ) ) ;
#17997 = CARTESIAN_POINT ( 'NONE',  ( -0.6781431574100000859, -62.17334590100000469, -148.5552959529999839 ) ) ;
#17998 = CARTESIAN_POINT ( 'NONE',  ( 31.32297112069999656, -40.18599471579999971, -149.5552959529999839 ) ) ;
#17999 = CARTESIAN_POINT ( 'NONE',  ( 7.663302333319010451, 38.24496471919625407, -141.8873347153860607 ) ) ;
#18000 = ORIENTED_EDGE ( 'NONE', *, *, #18880, .F. ) ;
#18001 = FILL_AREA_STYLE ('',( #20144 ) ) ;
#18002 = CARTESIAN_POINT ( 'NONE',  ( -19.95597284623131173, 34.08874935939712714, -140.3436463108538703 ) ) ;
#18003 = CARTESIAN_POINT ( 'NONE',  ( -8.554523812450000264, 40.80811760249999764, -146.2789059460000090 ) ) ;
#18004 = CARTESIAN_POINT ( 'NONE',  ( 8.201139657866018950, -31.10711941572444061, -136.0552959530184864 ) ) ;
#18005 = EDGE_LOOP ( 'NONE', ( #3388, #14155, #21955, #19657 ) ) ;
#18006 = CARTESIAN_POINT ( 'NONE',  ( -15.31679993919999916, -34.50000000000000000, -150.0552959529999839 ) ) ;
#18007 =( LENGTH_UNIT ( ) NAMED_UNIT ( * ) SI_UNIT ( .MILLI., .METRE. ) );
#18008 = APPLICATION_CONTEXT ( 'automotive_design' ) ;
#18009 = EDGE_CURVE ( 'NONE', #8753, #13874, #14252, .T. ) ;
#18010 = ORIENTED_EDGE ( 'NONE', *, *, #21448, .T. ) ;
#18011 = LINE ( 'NONE', #1836, #1991 ) ;
#18012 = CARTESIAN_POINT ( 'NONE',  ( -22.73109880829999696, 38.77532135890000120, -140.2559096070000066 ) ) ;
#18013 = CARTESIAN_POINT ( 'NONE',  ( 32.50000000000000000, -40.03620104880000241, -136.0552959519999945 ) ) ;
#18014 = ORIENTED_EDGE ( 'NONE', *, *, #12298, .T. ) ;
#18015 = DIRECTION ( 'NONE',  ( 0.000000000000000000, 0.000000000000000000, 1.000000000000000000 ) ) ;
#18016 = LINE ( 'NONE', #5514, #8725 ) ;
#18017 = VERTEX_POINT ( 'NONE', #12572 ) ;
#18018 = DIRECTION ( 'NONE',  ( 1.000000000000000000, -5.094701932209999624E-24, 0.000000000000000000 ) ) ;
#18019 = DIRECTION ( 'NONE',  ( -1.000000000000000000, 0.000000000000000000, 2.257120985840000117E-12 ) ) ;
#18020 = CARTESIAN_POINT ( 'NONE',  ( 13.13369214870000157, -51.50000000000000000, -137.0552959530000123 ) ) ;
#18021 = LINE ( 'NONE', #8720, #20158 ) ;
#18022 = FACE_OUTER_BOUND ( 'NONE', #9492, .T. ) ;
#18023 = CIRCLE ( 'NONE', #11926, 1.499999999999999556 ) ;
#18024 = DIRECTION ( 'NONE',  ( -1.000000000000000000, 0.000000000000000000, 2.257120985840000117E-12 ) ) ;
#18025 = CONTEXT_DEPENDENT_SHAPE_REPRESENTATION ( #20131, #13729 ) ;
#18026 = DIRECTION ( 'NONE',  ( -2.257144641399999941E-12, 8.049635416090000264E-35, -1.000000000000000000 ) ) ;
#18027 = CARTESIAN_POINT ( 'NONE',  ( 20.50000000000000000, 19.50000000000000000, -137.0552959530000123 ) ) ;
#18028 = PLANE ( 'NONE',  #7494 ) ;
#18029 = EDGE_CURVE ( 'NONE', #10073, #1168, #1889, .T. ) ;
#18030 = ORIENTED_EDGE ( 'NONE', *, *, #6716, .F. ) ;
#18031 = PRODUCT_DEFINITION_CONTEXT ( 'detailed design', #15264, 'design' ) ;
#18032 = VERTEX_POINT ( 'NONE', #12449 ) ;
#18033 = ADVANCED_FACE ( 'NONE', ( #12691, #3302 ), #8990, .T. ) ;
#18034 = ORIENTED_EDGE ( 'NONE', *, *, #22626, .T. ) ;
#18035 = CARTESIAN_POINT ( 'NONE',  ( 16.74346552629999962, -18.31657829129999726, -148.0552959529999839 ) ) ;
#18036 = CARTESIAN_POINT ( 'NONE',  ( -12.95309207247981753, 35.58606224187055744, -147.4460499723959970 ) ) ;
#18037 = LINE ( 'NONE', #1748, #22467 ) ;
#18038 = CARTESIAN_POINT ( 'NONE',  ( 13.24084097724100317, 23.82487805073530041, -136.0552959530298835 ) ) ;
#18039 = ORIENTED_EDGE ( 'NONE', *, *, #11192, .T. ) ;
#18040 = VECTOR ( 'NONE', #4779, 1000.000000000000000 ) ;
#18041 = CARTESIAN_POINT ( 'NONE',  ( 2.500000000170000014, 16.50000000000000000, -136.5552959530000123 ) ) ;
#18042 = CARTESIAN_POINT ( 'NONE',  ( -20.61753010269738340, 36.92891383027765784, -140.0927360959155976 ) ) ;
#18043 = CARTESIAN_POINT ( 'NONE',  ( -11.81646477902665637, 40.44164707346661913, -144.5342250517892353 ) ) ;
#18044 = LINE ( 'NONE', #10880, #9527 ) ;
#18045 = ORIENTED_EDGE ( 'NONE', *, *, #3134, .F. ) ;
#18046 = FACE_BOUND ( 'NONE', #13465, .T. ) ;
#18047 = ORIENTED_EDGE ( 'NONE', *, *, #4600, .T. ) ;
#18048 = CARTESIAN_POINT ( 'NONE',  ( 8.931951867280000457, -17.52729875919999714, -143.5552959529999839 ) ) ;
#18049 = EDGE_CURVE ( 'NONE', #4360, #17493, #16275, .T. ) ;
#18050 = CARTESIAN_POINT ( 'NONE',  ( -18.60901166351237279, 37.01038625230346923, -148.6497975989736346 ) ) ;
#18051 = DIRECTION ( 'NONE',  ( 0.7071067811865475727, -0.7071067811865475727, 0.000000000000000000 ) ) ;
#18052 = ORIENTED_EDGE ( 'NONE', *, *, #12597, .F. ) ;
#18053 = DIRECTION ( 'NONE',  ( 1.000000000000000000, 0.000000000000000000, 0.000000000000000000 ) ) ;
#18054 = ORIENTED_EDGE ( 'NONE', *, *, #21676, .T. ) ;
#18055 = CIRCLE ( 'NONE', #16911, 2.500000000000002220 ) ;
#18056 = CARTESIAN_POINT ( 'NONE',  ( -19.89002371299999794, 39.36161564540000057, -140.9617346340000381 ) ) ;
#18057 = CARTESIAN_POINT ( 'NONE',  ( -14.47770030809999930, -15.50000000000000000, -147.5552959529999839 ) ) ;
#18058 = ORIENTED_EDGE ( 'NONE', *, *, #16548, .T. ) ;
#18059 = CARTESIAN_POINT ( 'NONE',  ( 26.42191803000496009, -21.28524365307783484, -150.0552959530000123 ) ) ;
#18060 = ORIENTED_EDGE ( 'NONE', *, *, #10734, .T. ) ;
#18061 = EDGE_CURVE ( 'NONE', #18787, #14486, #20078, .T. ) ;
#18062 = CARTESIAN_POINT ( 'NONE',  ( -15.70137303715876875, 38.91953314721723700, -148.2523098871654383 ) ) ;
#18063 = DIRECTION ( 'NONE',  ( 1.000000000000000000, 0.000000000000000000, -4.429789868254374596E-12 ) ) ;
#18064 = ADVANCED_FACE ( 'NONE', ( #23296 ), #10660, .T. ) ;
#18065 = ORIENTED_EDGE ( 'NONE', *, *, #8488, .T. ) ;
#18066 = DIRECTION ( 'NONE',  ( 1.000000000000000000, 0.000000000000000000, 0.000000000000000000 ) ) ;
#18067 = ORIENTED_EDGE ( 'NONE', *, *, #13997, .F. ) ;
#18068 = CARTESIAN_POINT ( 'NONE',  ( -22.10824191589999899, -32.00000000000000000, -144.8157682189905984 ) ) ;
#18069 = PLANE ( 'NONE',  #12628 ) ;
#18070 = EDGE_LOOP ( 'NONE', ( #17080, #11767, #10124, #20298 ) ) ;
#18071 = CARTESIAN_POINT ( 'NONE',  ( -32.50000000000000000, -35.00000000000000000, -151.0552959529999839 ) ) ;
#18072 = DIRECTION ( 'NONE',  ( -0.9954742291034676116, 0.09503188512734456195, 0.000000000000000000 ) ) ;
#18073 = DIRECTION ( 'NONE',  ( 0.000000000000000000, -1.000000000000000000, 0.000000000000000000 ) ) ;
#18074 = ORIENTED_EDGE ( 'NONE', *, *, #21916, .F. ) ;
#18075 = CARTESIAN_POINT ( 'NONE',  ( -15.94523344369999940, 33.71216531379999282, -145.7766456660000074 ) ) ;
#18076 = AXIS2_PLACEMENT_3D ( 'NONE', #17528, #23354, #14306 ) ;
#18077 = VECTOR ( 'NONE', #3767, 1000.000000000000000 ) ;
#18078 = ORIENTED_EDGE ( 'NONE', *, *, #8046, .T. ) ;
#18079 = CARTESIAN_POINT ( 'NONE',  ( -4.499999999949999996, 31.50000000000000000, -150.0552959529999839 ) ) ;
#18080 = EDGE_CURVE ( 'NONE', #941, #22145, #11625, .T. ) ;
#18081 = CARTESIAN_POINT ( 'NONE',  ( -20.60824191589999899, -4.099603707729763791, -146.3157682190056619 ) ) ;
#18082 = CARTESIAN_POINT ( 'NONE',  ( -16.55827375307784877, 37.05535324330323732, -139.5705083843519390 ) ) ;
#18083 = LINE ( 'NONE', #9015, #20132 ) ;
#18084 = VERTEX_POINT ( 'NONE', #6990 ) ;
#18085 =( NAMED_UNIT ( * ) SI_UNIT ( $, .STERADIAN. ) SOLID_ANGLE_UNIT ( ) );
#18086 = CARTESIAN_POINT ( 'NONE',  ( -34.61111111099999960, 47.50000000000000000, -140.5552959529999839 ) ) ;
#18087 = DIRECTION ( 'NONE',  ( 1.000000000000000000, 0.000000000000000000, -2.257453483404482811E-12 ) ) ;
#18088 = DIRECTION ( 'NONE',  ( 0.000000000000000000, -1.000000000000000000, 0.000000000000000000 ) ) ;
#18089 = DIRECTION ( 'NONE',  ( 0.000000000000000000, 0.8775825618903703162, 0.4794255386042076128 ) ) ;
#18090 = DIRECTION ( 'NONE',  ( 1.526468026909999897E-13, 8.159623473500000156E-13, 1.000000000000000000 ) ) ;
#18091 = VECTOR ( 'NONE', #23324, 1000.000000000000000 ) ;
#18092 = EDGE_CURVE ( 'NONE', #3905, #21024, #16158, .T. ) ;
#18093 = VECTOR ( 'NONE', #21925, 1000.000000000000000 ) ;
#18094 = ORIENTED_EDGE ( 'NONE', *, *, #199, .T. ) ;
#18095 = DIRECTION ( 'NONE',  ( 0.000000000000000000, 1.000000000000000000, 0.000000000000000000 ) ) ;
#18096 = DIRECTION ( 'NONE',  ( 2.257305453670000045E-12, 0.000000000000000000, 1.000000000000000000 ) ) ;
#18097 = CARTESIAN_POINT ( 'NONE',  ( 2.656359840075261047, -5.899000527194546706, -150.0552959529999839 ) ) ;
#18098 = CARTESIAN_POINT ( 'NONE',  ( -5.136302089049142872, 41.25620344490214819, -143.6246837869908575 ) ) ;
#18099 = CARTESIAN_POINT ( 'NONE',  ( -9.334216945200001447, -17.19633444960000190, -145.5552959529999839 ) ) ;
#18100 = ORIENTED_EDGE ( 'NONE', *, *, #7618, .T. ) ;
#18101 = FACE_OUTER_BOUND ( 'NONE', #18149, .T. ) ;
#18102 = ADVANCED_FACE ( 'NONE', ( #14493 ), #17943, .T. ) ;
#18103 = CARTESIAN_POINT ( 'NONE',  ( -31.75000000000000000, 1.000000000000000000, -151.0552959529999839 ) ) ;
#18104 = VERTEX_POINT ( 'NONE', #12802 ) ;
#18105 = AXIS2_PLACEMENT_3D ( 'NONE', #13583, #8106, #22636 ) ;
#18106 = CARTESIAN_POINT ( 'NONE',  ( 3.298969449361869088, -2.579871919192233687, -136.0552959530074872 ) ) ;
#18107 = EDGE_LOOP ( 'NONE', ( #6813, #20621, #14086, #9210 ) ) ;
#18108 = LINE ( 'NONE', #16327, #15159 ) ;
#18109 = ADVANCED_FACE ( 'NONE', ( #5446 ), #21760, .F. ) ;
#18110 = CARTESIAN_POINT ( 'NONE',  ( -29.82391180389999619, 40.55477172079999804, -144.2881336360000262 ) ) ;
#18111 = EDGE_CURVE ( 'NONE', #22981, #7563, #16392, .T. ) ;
#18112 = CARTESIAN_POINT ( 'NONE',  ( -32.50000000000000000, 48.75000000000000000, -151.0552959529999839 ) ) ;
#18113 = CARTESIAN_POINT ( 'NONE',  ( 7.085192309373985253, 36.50051581081366692, -141.6055286362093000 ) ) ;
#18114 = ORIENTED_EDGE ( 'NONE', *, *, #21890, .T. ) ;
#18115 = CARTESIAN_POINT ( 'NONE',  ( -34.50000000000000000, 67.50000000000000000, -144.0552959529999839 ) ) ;
#18116 = CARTESIAN_POINT ( 'NONE',  ( -20.34672008420000111, 36.01786665889999739, -139.8153362750000213 ) ) ;
#18117 = EDGE_CURVE ( 'NONE', #2929, #14604, #14603, .T. ) ;
#18118 = CARTESIAN_POINT ( 'NONE',  ( -9.197324267974639866, 40.96642299190880010, -143.5436038169824258 ) ) ;
#18119 = CARTESIAN_POINT ( 'NONE',  ( 5.569521322453342194, -30.97557888555125771, -136.0552959530125463 ) ) ;
#18120 = EDGE_CURVE ( 'NONE', #13663, #2031, #3043, .T. ) ;
#18121 = VERTEX_POINT ( 'NONE', #8718 ) ;
#18122 = CARTESIAN_POINT ( 'NONE',  ( 20.50000000000000000, 19.50000000000000000, -136.0552959530000123 ) ) ;
#18123 = ORIENTED_EDGE ( 'NONE', *, *, #21262, .F. ) ;
#18124 = AXIS2_PLACEMENT_3D ( 'NONE', #3628, #18026, #16245 ) ;
#18125 = DIRECTION ( 'NONE',  ( 0.000000000000000000, -1.000000000000000000, 3.568879590630000244E-13 ) ) ;
#18126 = CARTESIAN_POINT ( 'NONE',  ( -25.85824191589999899, -34.50000000000000000, -144.8157682190000060 ) ) ;
#18127 = DIRECTION ( 'NONE',  ( 4.430318231639999944E-12, -6.100259101500000139E-13, 1.000000000000000000 ) ) ;
#18128 = ORIENTED_EDGE ( 'NONE', *, *, #11548, .F. ) ;
#18129 = CARTESIAN_POINT ( 'NONE',  ( -17.08912089869999917, -1.500000000000000000, -147.1421200419999877 ) ) ;
#18130 = CARTESIAN_POINT ( 'NONE',  ( 23.41308733940000053, -15.43505800149999985, -148.0552959529999839 ) ) ;
#18131 = EDGE_LOOP ( 'NONE', ( #5339, #15463, #11149, #3705 ) ) ;
#18132 = ADVANCED_FACE ( 'NONE', ( #15871 ), #3160, .T. ) ;
#18133 = DIRECTION ( 'NONE',  ( -0.09606172499277226828, -0.9953753789357124848, 8.289665250527615055E-13 ) ) ;
#18134 = LINE ( 'NONE', #7183, #14019 ) ;
#18135 = CARTESIAN_POINT ( 'NONE',  ( 16.87269471589999981, -31.91616505980000085, -144.5552959529999839 ) ) ;
#18136 = CARTESIAN_POINT ( 'NONE',  ( 32.50000000000000000, -27.03620104879999886, -137.0552959530000123 ) ) ;
#18137 = VECTOR ( 'NONE', #18024, 1000.000000000000000 ) ;
#18138 = EDGE_CURVE ( 'NONE', #17964, #2277, #19206, .T. ) ;
#18139 = DIRECTION ( 'NONE',  ( 1.000000000000000000, 0.000000000000000000, 0.000000000000000000 ) ) ;
#18140 = EDGE_CURVE ( 'NONE', #20358, #14413, #9347, .T. ) ;
#18141 = STYLED_ITEM ( 'NONE', ( #1711 ), #19431 ) ;
#18142 = CARTESIAN_POINT ( 'NONE',  ( -4.499999999969999109, 34.00000000000000000, -136.5552959530000123 ) ) ;
#18143 = CONTEXT_DEPENDENT_SHAPE_REPRESENTATION ( #10686, #2888 ) ;
#18144 = CARTESIAN_POINT ( 'NONE',  ( 23.84377886109999878, -30.60602870049999780, -145.5552959529999839 ) ) ;
#18145 = DIRECTION ( 'NONE',  ( 2.257083409060000051E-12, 0.000000000000000000, 1.000000000000000000 ) ) ;
#18146 = DIRECTION ( 'NONE',  ( 0.000000000000000000, -1.000000000000000000, 1.723073263340000007E-12 ) ) ;
#18147 = ORIENTED_EDGE ( 'NONE', *, *, #10682, .F. ) ;
#18148 = ORIENTED_EDGE ( 'NONE', *, *, #16157, .F. ) ;
#18149 = EDGE_LOOP ( 'NONE', ( #15307, #5357, #7392, #5552 ) ) ;
#18150 = PLANE ( 'NONE',  #4531 ) ;
#18151 = CARTESIAN_POINT ( 'NONE',  ( -13.11071995283477953, 37.07027326795081734, -147.8134892432882452 ) ) ;
#18152 = EDGE_LOOP ( 'NONE', ( #15632, #10883, #11158, #20764 ) ) ;
#18153 = CARTESIAN_POINT ( 'NONE',  ( 12.15117705468384202, 25.45516771069291195, -136.0552959530274677 ) ) ;
#18154 = CIRCLE ( 'NONE', #2577, 5.000000000000000000 ) ;
#18155 = ORIENTED_EDGE ( 'NONE', *, *, #6046, .T. ) ;
#18156 = CARTESIAN_POINT ( 'NONE',  ( -6.719053507402335867, 25.42349012523258267, -150.0552959530000123 ) ) ;
#18157 = CARTESIAN_POINT ( 'NONE',  ( -19.59117934188227395, 33.37909977088141744, -146.4170658873010495 ) ) ;
#18158 = VECTOR ( 'NONE', #703, 1000.000000000000227 ) ;
#18159 = CARTESIAN_POINT ( 'NONE',  ( -11.16766646727579015, 41.31356556668690416, -143.7956700918360298 ) ) ;
#18160 = CARTESIAN_POINT ( 'NONE',  ( -32.50000000000000000, -50.00000000000000000, -143.3052959529999839 ) ) ;
#18161 = ORIENTED_EDGE ( 'NONE', *, *, #16233, .F. ) ;
#18162 = FACE_BOUND ( 'NONE', #3198, .T. ) ;
#18163 = ORIENTED_EDGE ( 'NONE', *, *, #22462, .F. ) ;
#18164 = CARTESIAN_POINT ( 'NONE',  ( 8.598996733729995512, 35.50242794714858263, -142.0534435078296269 ) ) ;
#18165 = EDGE_CURVE ( 'NONE', #2447, #11281, #6595, .T. ) ;
#18166 = CARTESIAN_POINT ( 'NONE',  ( -2.499999999920000437, 37.00000000000000000, -135.0552959530000123 ) ) ;
#18167 = LINE ( 'NONE', #16031, #17465 ) ;
#18168 = ORIENTED_EDGE ( 'NONE', *, *, #18257, .F. ) ;
#18169 = VECTOR ( 'NONE', #1445, 1000.000000000000000 ) ;
#18170 = DIRECTION ( 'NONE',  ( 1.000000000000000000, 0.000000000000000000, -2.257171095940000041E-12 ) ) ;
#18171 =( GEOMETRIC_REPRESENTATION_CONTEXT ( 3 ) GLOBAL_UNCERTAINTY_ASSIGNED_CONTEXT ( ( #10633 ) ) GLOBAL_UNIT_ASSIGNED_CONTEXT ( ( #16607, #12923, #5896 ) ) REPRESENTATION_CONTEXT ( 'NONE', 'WORKASPACE' ) );
#18172 = VERTEX_POINT ( 'NONE', #19573 ) ;
#18173 = CARTESIAN_POINT ( 'NONE',  ( -2.499999999839999987, 20.50000000000000000, -140.0552959529999839 ) ) ;
#18174 = DIRECTION ( 'NONE',  ( 1.000000000000000000, 0.000000000000000000, 0.000000000000000000 ) ) ;
#18175 = ORIENTED_EDGE ( 'NONE', *, *, #12272, .F. ) ;
#18176 = CARTESIAN_POINT ( 'NONE',  ( -25.74743564712004229, 37.94517732367248186, -139.7356315992777809 ) ) ;
#18177 = ORIENTED_EDGE ( 'NONE', *, *, #14942, .F. ) ;
#18178 = CARTESIAN_POINT ( 'NONE',  ( 2.508811538190000245, -14.35090895149999923, -145.5552959529999839 ) ) ;
#18179 = CARTESIAN_POINT ( 'NONE',  ( 19.45666326950000169, -50.88169314249999786, -149.5552959529999839 ) ) ;
#18180 = VERTEX_POINT ( 'NONE', #13972 ) ;
#18181 = FILL_AREA_STYLE_COLOUR ( '', #17225 ) ;
#18182 = ORIENTED_EDGE ( 'NONE', *, *, #10866, .F. ) ;
#18183 = CARTESIAN_POINT ( 'NONE',  ( -45.83792946319999828, 37.00000000000000000, -146.9594324700000243 ) ) ;
#18184 = LINE ( 'NONE', #16049, #14546 ) ;
#18185 = ORIENTED_EDGE ( 'NONE', *, *, #8654, .F. ) ;
#18186 = DIRECTION ( 'NONE',  ( 2.257144641399999941E-12, -8.049635416090000264E-35, 1.000000000000000000 ) ) ;
#18187 = CARTESIAN_POINT ( 'NONE',  ( -10.92854443057495928, 33.70908472042151516, -142.0058283512219930 ) ) ;
#18188 = AXIS2_PLACEMENT_3D ( 'NONE', #17010, #4398, #9856 ) ;
#18189 = VECTOR ( 'NONE', #19117, 1000.000000000000227 ) ;
#18190 = DIRECTION ( 'NONE',  ( -0.7633862853691523176, -0.6459422414661291079, 0.000000000000000000 ) ) ;
#18191 = ORIENTED_EDGE ( 'NONE', *, *, #15208, .F. ) ;
#18192 = VECTOR ( 'NONE', #1332, 1000.000000000000000 ) ;
#18193 = LINE ( 'NONE', #1788, #12478 ) ;
#18194 = EDGE_CURVE ( 'NONE', #19589, #18962, #17776, .T. ) ;
#18195 = LINE ( 'NONE', #22119, #10593 ) ;
#18196 = VECTOR ( 'NONE', #18527, 1000.000000000000000 ) ;
#18197 = EDGE_CURVE ( 'NONE', #258, #23250, #15762, .T. ) ;
#18198 = ORIENTED_EDGE ( 'NONE', *, *, #15933, .F. ) ;
#18199 = CARTESIAN_POINT ( 'NONE',  ( -34.50000000000000000, 48.00000000000000000, -146.5552959529999839 ) ) ;
#18200 = CARTESIAN_POINT ( 'NONE',  ( -24.00000000000000000, 47.50000000000000000, -137.0552959530000123 ) ) ;
#18201 = CARTESIAN_POINT ( 'NONE',  ( 9.683200060759999062, -20.50000000000000000, -148.5552959529999839 ) ) ;
#18202 = CARTESIAN_POINT ( 'NONE',  ( -29.64895016830000429, 40.48034887659999725, -142.7934167989999992 ) ) ;
#18203 = ORIENTED_EDGE ( 'NONE', *, *, #7457, .F. ) ;
#18204 = CARTESIAN_POINT ( 'NONE',  ( 2.742326387988431424, 13.99062889862883097, -136.0552959530062083 ) ) ;
#18205 = PLANE ( 'NONE',  #12379 ) ;
#18206 = VECTOR ( 'NONE', #6383, 1000.000000000000000 ) ;
#18207 = PLANE ( 'NONE',  #789 ) ;
#18208 = CARTESIAN_POINT ( 'NONE',  ( -34.47299999999999898, 14.00000000000000000, -144.0552959529999839 ) ) ;
#18209 = CARTESIAN_POINT ( 'NONE',  ( 32.50000000000000000, -33.03620104880000241, -136.5552959530000123 ) ) ;
#18210 = CARTESIAN_POINT ( 'NONE',  ( 23.49999999970000175, -20.50000000000000000, -148.5552959529999839 ) ) ;
#18211 = VECTOR ( 'NONE', #23111, 1000.000000000000000 ) ;
#18212 = EDGE_LOOP ( 'NONE', ( #12019, #18536, #3083, #21260 ) ) ;
#18213 = CARTESIAN_POINT ( 'NONE',  ( 4.750000000000000000, -38.23606797749999942, -150.0552959529999839 ) ) ;
#18214 = VECTOR ( 'NONE', #17863, 1000.000000000000000 ) ;
#18215 = CYLINDRICAL_SURFACE ( 'NONE', #1173, 1.500000000000001110 ) ;
#18216 = AXIS2_PLACEMENT_3D ( 'NONE', #6453, #15618, #6799 ) ;
#18217 = DIRECTION ( 'NONE',  ( 0.000000000000000000, 0.000000000000000000, 1.000000000000000000 ) ) ;
#18218 = CARTESIAN_POINT ( 'NONE',  ( -5.733381482170000432, 39.34803470290000149, -147.3316303149999840 ) ) ;
#18219 = DIRECTION ( 'NONE',  ( 8.955190032050000935E-12, -9.104778821549999739E-13, 1.000000000000000000 ) ) ;
#18220 = ORIENTED_EDGE ( 'NONE', *, *, #21785, .F. ) ;
#18221 = LINE ( 'NONE', #10939, #11338 ) ;
#18222 = DIRECTION ( 'NONE',  ( 1.000000000000000000, 0.000000000000000000, 0.000000000000000000 ) ) ;
#18223 = ORIENTED_EDGE ( 'NONE', *, *, #14577, .T. ) ;
#18224 = PRODUCT ( 'Deadbolt', 'Deadbolt', '', ( #10624 ) ) ;
#18225 = VECTOR ( 'NONE', #18369, 1000.000000000000000 ) ;
#18226 = VECTOR ( 'NONE', #9482, 1000.000000000000000 ) ;
#18227 = ADVANCED_FACE ( 'NONE', ( #4937 ), #12183, .F. ) ;
#18228 = CARTESIAN_POINT ( 'NONE',  ( 4.300767767059650026, -1.999999999999999556, -136.0552959530097041 ) ) ;
#18229 = ORIENTED_EDGE ( 'NONE', *, *, #21701, .F. ) ;
#18230 = VECTOR ( 'NONE', #11142, 1000.000000000000000 ) ;
#18231 = CARTESIAN_POINT ( 'NONE',  ( -24.68730002459999895, 39.33688142210000649, -147.2285014869999884 ) ) ;
#18232 = CARTESIAN_POINT ( 'NONE',  ( -29.36832786400000117, 38.86294434210000048, -140.8528603229999874 ) ) ;
#18233 = AXIS2_PLACEMENT_3D ( 'NONE', #16763, #7481, #22130 ) ;
#18234 = AXIS2_PLACEMENT_3D ( 'NONE', #20246, #2160, #15235 ) ;
#18235 = CARTESIAN_POINT ( 'NONE',  ( 13.13369214870000157, -51.00000000000000000, -137.0552959530000123 ) ) ;
#18236 = CARTESIAN_POINT ( 'NONE',  ( 8.177875869394885200, 35.53494891409558676, -142.0295714736785442 ) ) ;
#18237 = VERTEX_POINT ( 'NONE', #1373 ) ;
#18238 =( LENGTH_UNIT ( ) NAMED_UNIT ( * ) SI_UNIT ( .MILLI., .METRE. ) );
#18239 = CARTESIAN_POINT ( 'NONE',  ( -19.04867772230000256, 35.29145880730000329, -148.2212826610000036 ) ) ;
#18240 = PRODUCT_RELATED_PRODUCT_CATEGORY ( 'part', '', ( #5209 ) ) ;
#18241 = CARTESIAN_POINT ( 'NONE',  ( 3.999999999879999546, -3.500000000000000000, -135.4552959529999896 ) ) ;
#18242 = CARTESIAN_POINT ( 'NONE',  ( 4.055709778280034428, -32.39604587945242997, -136.0552959530091641 ) ) ;
#18243 = CARTESIAN_POINT ( 'NONE',  ( -23.61758233950000019, 37.78045452579999619, -140.0909254550000185 ) ) ;
#18244 = EDGE_CURVE ( 'NONE', #6936, #16928, #8597, .T. ) ;
#18245 = CARTESIAN_POINT ( 'NONE',  ( 4.500000000009999113, -5.000000000000000000, -136.0552959530000123 ) ) ;
#18246 = DIRECTION ( 'NONE',  ( 0.000000000000000000, -1.000000000000000000, 0.000000000000000000 ) ) ;
#18247 = LINE ( 'NONE', #2308, #19069 ) ;
#18248 = CARTESIAN_POINT ( 'NONE',  ( -5.985028652370273150, 19.88109793996622443, -136.0552959529864552 ) ) ;
#18249 = AXIS2_PLACEMENT_3D ( 'NONE', #17658, #21471, #18015 ) ;
#18250 = ADVANCED_FACE ( 'NONE', ( #15522 ), #23259, .F. ) ;
#18251 = ORIENTED_EDGE ( 'NONE', *, *, #10866, .T. ) ;
#18252 = AXIS2_PLACEMENT_3D ( 'NONE', #18302, #2017, #9582 ) ;
#18253 = CARTESIAN_POINT ( 'NONE',  ( -5.762834417994439740, 39.50865942498580097, -140.4825946862647754 ) ) ;
#18254 = AXIS2_PLACEMENT_3D ( 'NONE', #21652, #6882, #12343 ) ;
#18255 = EDGE_LOOP ( 'NONE', ( #1910, #16340, #15689, #17035 ) ) ;
#18256 = DIRECTION ( 'NONE',  ( 0.000000000000000000, 0.000000000000000000, 1.000000000000000000 ) ) ;
#18257 = EDGE_CURVE ( 'NONE', #7545, #20852, #8833, .T. ) ;
#18258 = B_SPLINE_CURVE_WITH_KNOTS ( 'NONE', 3,
 ( #21577, #6810, #5259, #14077, #5037, #3140, #13841, #22894, #23238, #8695, #19190, #17646, #19552, #6692, #12388, #2900, #13951, #15628 ),
 .UNSPECIFIED., .F., .F.,
 ( 4, 2, 2, 2, 2, 2, 2, 2, 4 ),
 ( 0.000000000000000000, 0.1250000000000000000, 0.2500000000000000000, 0.3750000000000000000, 0.5000000000000000000, 0.6250000000000000000, 0.7500000000000000000, 0.8750000000000000000, 1.000000000000000000 ),
 .UNSPECIFIED. ) ;
#18259 = CARTESIAN_POINT ( 'NONE',  ( 8.750000000000000000, -44.61803398880000060, -151.0552959529999839 ) ) ;
#18260 = CARTESIAN_POINT ( 'NONE',  ( -38.39535039439999764, 29.00000000000000000, -147.5552959529999839 ) ) ;
#18261 = DIRECTION ( 'NONE',  ( 1.561251128379126385E-14, 1.000000000000000000, 0.000000000000000000 ) ) ;
#18262 = DIRECTION ( 'NONE',  ( -1.457881434619999915E-12, 1.723066134219999902E-12, 1.000000000000000000 ) ) ;
#18263 = CARTESIAN_POINT ( 'NONE',  ( 15.50000000000000000, 33.50000000000000000, -150.0552959529999839 ) ) ;
#18264 = APPLICATION_PROTOCOL_DEFINITION ( 'draft international standard', 'automotive_design', 1998, #17233 ) ;
#18265 = CARTESIAN_POINT ( 'NONE',  ( 4.499999999879999102, -5.500000000000000000, -143.0552959529999839 ) ) ;
#18266 = VECTOR ( 'NONE', #16771, 1000.000000000000000 ) ;
#18267 = CARTESIAN_POINT ( 'NONE',  ( 3.552713678799999608E-15, 50.00000000000000000, -149.5552959529999839 ) ) ;
#18268 = CARTESIAN_POINT ( 'NONE',  ( -13.36469768600054486, 37.07845968427643157, -139.9331372610153608 ) ) ;
#18269 = EDGE_CURVE ( 'NONE', #16883, #1705, #10803, .T. ) ;
#18270 = ORIENTED_EDGE ( 'NONE', *, *, #15631, .T. ) ;
#18271 = UNCERTAINTY_MEASURE_WITH_UNIT (LENGTH_MEASURE( 1.000000000000000082E-05 ), #18596, 'distance_accuracy_value', 'NONE');
#18272 = EDGE_CURVE ( 'NONE', #13979, #13387, #1967, .T. ) ;
#18273 = VERTEX_POINT ( 'NONE', #1622 ) ;
#18274 = VERTEX_POINT ( 'NONE', #7308 ) ;
#18275 = CARTESIAN_POINT ( 'NONE',  ( -16.23340181981567198, 34.21381099665894965, -147.7313700749976988 ) ) ;
#18276 = CARTESIAN_POINT ( 'NONE',  ( 4.999999999879999990, -5.500000000000000000, -135.2552959529999725 ) ) ;
#18277 = ORIENTED_EDGE ( 'NONE', *, *, #12566, .F. ) ;
#18278 = DIRECTION ( 'NONE',  ( 0.000000000000000000, 0.000000000000000000, 1.000000000000000000 ) ) ;
#18279 = EDGE_CURVE ( 'NONE', #12078, #5331, #16465, .T. ) ;
#18280 = VERTEX_POINT ( 'NONE', #12884 ) ;
#18281 = FACE_OUTER_BOUND ( 'NONE', #9552, .T. ) ;
#18282 = CARTESIAN_POINT ( 'NONE',  ( -19.38998902330187590, 34.64861313674464327, -147.6078979941154898 ) ) ;
#18283 = ADVANCED_FACE ( 'NONE', ( #5746 ), #12530, .F. ) ;
#18284 = LINE ( 'NONE', #192, #6778 ) ;
#18285 = ORIENTED_EDGE ( 'NONE', *, *, #4982, .T. ) ;
#18286 = COLOUR_RGB ( '', 0.31764706, 0.68627451, 0.89019608) ;
#18287 = FACE_OUTER_BOUND ( 'NONE', #12928, .T. ) ;
#18288 = EDGE_CURVE ( 'NONE', #10060, #11714, #10867, .T. ) ;
#18289 = EDGE_LOOP ( 'NONE', ( #15567, #11956, #17513, #16397 ) ) ;
#18290 = CARTESIAN_POINT ( 'NONE',  ( 8.699041270020327232, 38.49025597642661722, -142.0478759868930183 ) ) ;
#18291 = DIRECTION ( 'NONE',  ( -0.8571428571427679444, -0.5150787536378610421, 1.934960128632415569E-12 ) ) ;
#18292 = CARTESIAN_POINT ( 'NONE',  ( -27.26567793380000282, 36.96940380710000085, -148.4835048639999968 ) ) ;
#18293 = VERTEX_POINT ( 'NONE', #5518 ) ;
#18294 = LINE ( 'NONE', #3656, #17904 ) ;
#18295 = ORIENTED_EDGE ( 'NONE', *, *, #16843, .T. ) ;
#18296 = LINE ( 'NONE', #14709, #22735 ) ;
#18297 = CIRCLE ( 'NONE', #12971, 7.499999999999999112 ) ;
#18298 = ORIENTED_EDGE ( 'NONE', *, *, #20170, .T. ) ;
#18299 = CARTESIAN_POINT ( 'NONE',  ( -26.17844700321043661, 36.98132551455271511, -140.6351982806931176 ) ) ;
#18300 = EDGE_LOOP ( 'NONE', ( #19997, #3778, #13960 ) ) ;
#18301 = CARTESIAN_POINT ( 'NONE',  ( -21.77251801933481445, 32.71408580851625203, -146.4208751718306303 ) ) ;
#18302 = CARTESIAN_POINT ( 'NONE',  ( -44.50000000000000000, 26.50000000000000000, -148.4460207619999892 ) ) ;
#18303 = ORIENTED_EDGE ( 'NONE', *, *, #19941, .T. ) ;
#18304 = PRODUCT_CONTEXT ( 'NONE', #13127, 'mechanical' ) ;
#18305 = ORIENTED_EDGE ( 'NONE', *, *, #19412, .F. ) ;
#18306 = CARTESIAN_POINT ( 'NONE',  ( -26.61369313923914603, 36.92937183404335855, -140.1328975134355517 ) ) ;
#18307 = DIRECTION ( 'NONE',  ( -0.9919007982877544594, 0.1270149847699686418, 4.766005912188822159E-14 ) ) ;
#18308 = EDGE_CURVE ( 'NONE', #13529, #12052, #19234, .T. ) ;
#18309 = CARTESIAN_POINT ( 'NONE',  ( -7.500000000000000000, 25.50000000000000000, -151.0552959529999839 ) ) ;
#18310 = CARTESIAN_POINT ( 'NONE',  ( -6.166004029541132248, 36.95750611116266526, -148.6250205690584778 ) ) ;
#18311 = CARTESIAN_POINT ( 'NONE',  ( -11.10890527118989901, 34.84141842858843319, -140.9538660573311972 ) ) ;
#18312 = FACE_OUTER_BOUND ( 'NONE', #14620, .T. ) ;
#18313 = VERTEX_POINT ( 'NONE', #20165 ) ;
#18314 = LINE ( 'NONE', #19751, #12875 ) ;
#18315 = AXIS2_PLACEMENT_3D ( 'NONE', #21580, #23470, #7165 ) ;
#18316 = VECTOR ( 'NONE', #627, 1000.000000000000114 ) ;
#18317 = AXIS2_PLACEMENT_3D ( 'NONE', #17151, #9753, #15014 ) ;
#18318 = LINE ( 'NONE', #9475, #19747 ) ;
#18319 = ORIENTED_EDGE ( 'NONE', *, *, #2044, .F. ) ;
#18320 = DIRECTION ( 'NONE',  ( 0.000000000000000000, 0.000000000000000000, -1.000000000000000000 ) ) ;
#18321 = CARTESIAN_POINT ( 'NONE',  ( -31.75000000030000180, -51.50000000000000000, -149.5552959529999839 ) ) ;
#18322 = CARTESIAN_POINT ( 'NONE',  ( -17.44989882376803791, 40.67283837537863889, -143.6255418396287666 ) ) ;
#18323 = CARTESIAN_POINT ( 'NONE',  ( -29.21069264103822150, 41.10559376373601737, -145.0521024197723818 ) ) ;
#18324 = ORIENTED_EDGE ( 'NONE', *, *, #23496, .T. ) ;
#18325 = LINE ( 'NONE', #2037, #20822 ) ;
#18326 = CARTESIAN_POINT ( 'NONE',  ( -6.683153925719999222, 51.50000000000000000, -136.0552959530000123 ) ) ;
#18327 = FACE_BOUND ( 'NONE', #4710, .T. ) ;
#18328 = DIRECTION ( 'NONE',  ( -1.211690350419999855E-27, -2.765629237170000203E-27, 1.000000000000000000 ) ) ;
#18329 = DIRECTION ( 'NONE',  ( 0.9834926989016489207, 0.1809478134909354718, -4.411697319228424767E-12 ) ) ;
#18330 = CARTESIAN_POINT ( 'NONE',  ( 20.58976242830000203, -31.80400447969999789, -143.5552959529999839 ) ) ;
#18331 = CIRCLE ( 'NONE', #2373, 4.000000000000000000 ) ;
#18332 = ORIENTED_EDGE ( 'NONE', *, *, #6691, .T. ) ;
#18333 = ADVANCED_FACE ( 'NONE', ( #14327 ), #18370, .F. ) ;
#18334 = AXIS2_PLACEMENT_3D ( 'NONE', #13083, #6407, #19259 ) ;
#18335 = LINE ( 'NONE', #2395, #20535 ) ;
#18336 = EDGE_CURVE ( 'NONE', #20005, #7769, #23373, .T. ) ;
#18337 = DIRECTION ( 'NONE',  ( -0.04567108003750790929, 0.9989565318111732761, -8.081393722541401004E-13 ) ) ;
#18338 = CARTESIAN_POINT ( 'NONE',  ( -5.932764524189999555, 37.76833845600000217, -147.9772051180000005 ) ) ;
#18339 = EDGE_CURVE ( 'NONE', #9011, #14876, #16205, .T. ) ;
#18340 = LINE ( 'NONE', #5370, #7763 ) ;
#18341 = VERTEX_POINT ( 'NONE', #18020 ) ;
#18342 = DIRECTION ( 'NONE',  ( 0.000000000000000000, 8.018988631039999700E-27, -1.000000000000000000 ) ) ;
#18343 = DIRECTION ( 'NONE',  ( 0.000000000000000000, -3.386627385143914456E-17, -1.000000000000000000 ) ) ;
#18344 = VERTEX_POINT ( 'NONE', #9298 ) ;
#18345 = ADVANCED_BREP_SHAPE_REPRESENTATION ( '', ( #11693, #5025 ), #14199 ) ;
#18346 = STYLED_ITEM ( 'NONE', ( #23362 ), #19731 ) ;
#18347 = ORIENTED_EDGE ( 'NONE', *, *, #21864, .T. ) ;
#18348 = VECTOR ( 'NONE', #752, 1000.000000000000000 ) ;
#18349 = DIRECTION ( 'NONE',  ( -0.09606172499277228216, -0.9953753789357123738, 8.282644157540153068E-13 ) ) ;
#18350 = CARTESIAN_POINT ( 'NONE',  ( 1.133692148550000001, -51.00000000000000000, -136.0552959530000123 ) ) ;
#18351 = CARTESIAN_POINT ( 'NONE',  ( 5.347956485829999274, -22.34165470570000167, -147.5552959529999839 ) ) ;
#18352 = DIRECTION ( 'NONE',  ( 0.000000000000000000, -1.000000000000000000, 0.000000000000000000 ) ) ;
#18353 = ORIENTED_EDGE ( 'NONE', *, *, #5237, .F. ) ;
#18354 =( NAMED_UNIT ( * ) SI_UNIT ( $, .STERADIAN. ) SOLID_ANGLE_UNIT ( ) );
#18355 = CARTESIAN_POINT ( 'NONE',  ( -17.98984244384617526, 36.14647386681518526, -147.9375626265034498 ) ) ;
#18356 = CARTESIAN_POINT ( 'NONE',  ( -31.00000000000000000, 19.50000000000000000, -151.0552959529999839 ) ) ;
#18357 = DIRECTION ( 'NONE',  ( -0.1739442350240419932, -0.9847555042252370550, 8.300754441162000146E-13 ) ) ;
#18358 = CARTESIAN_POINT ( 'NONE',  ( -13.86630785140000022, -50.50000000000000000, -136.0552959530000123 ) ) ;
#18359 = CARTESIAN_POINT ( 'NONE',  ( -15.17576278497271502, 36.16931166175189105, -147.5919646919771822 ) ) ;
#18360 = EDGE_CURVE ( 'NONE', #6393, #7102, #1732, .T. ) ;
#18361 = DIRECTION ( 'NONE',  ( 2.839308199620000013E-14, 3.568879590630000244E-13, 1.000000000000000000 ) ) ;
#18362 = CARTESIAN_POINT ( 'NONE',  ( -9.434278515689999978, -18.41834002140000237, -147.5552959529999839 ) ) ;
#18363 = EDGE_CURVE ( 'NONE', #7276, #9232, #18472, .T. ) ;
#18364 = DIRECTION ( 'NONE',  ( -0.09503188512734457583, -0.9954742291034677226, 2.970706163671393545E-13 ) ) ;
#18365 = ORIENTED_EDGE ( 'NONE', *, *, #3234, .T. ) ;
#18366 = CARTESIAN_POINT ( 'NONE',  ( -6.804059094464567359, 37.03366832433017208, -147.4295713063914377 ) ) ;
#18367 = ORIENTED_EDGE ( 'NONE', *, *, #303, .T. ) ;
#18368 = CARTESIAN_POINT ( 'NONE',  ( -12.50000000000000000, 42.50000000000000000, -136.5552959530000123 ) ) ;
#18369 = DIRECTION ( 'NONE',  ( 0.000000000000000000, -1.000000000000000000, 0.000000000000000000 ) ) ;
#18370 = PLANE ( 'NONE',  #21922 ) ;
#18371 = CARTESIAN_POINT ( 'NONE',  ( -24.97797643630000053, 37.05442817780000553, -147.8575004449999994 ) ) ;
#18372 = CARTESIAN_POINT ( 'NONE',  ( -13.38748872365634135, 33.38537881988771971, -144.5933708985054125 ) ) ;
#18373 = CARTESIAN_POINT ( 'NONE',  ( -32.50000000000000000, 19.50000000000000000, -143.3052959529999839 ) ) ;
#18374 = CARTESIAN_POINT ( 'NONE',  ( -32.50000000000000000, 37.00000000000000000, -150.5552959529999839 ) ) ;
#18375 = DIRECTION ( 'NONE',  ( 1.000000000000000000, 0.000000000000000000, 2.257144641399999941E-12 ) ) ;
#18376 = DIRECTION ( 'NONE',  ( 0.000000000000000000, 1.000000000000000000, 0.000000000000000000 ) ) ;
#18377 = EDGE_CURVE ( 'NONE', #13765, #751, #9067, .T. ) ;
#18378 = CARTESIAN_POINT ( 'NONE',  ( 4.500000000009999113, -5.000000000000000000, -136.0552959530000123 ) ) ;
#18379 = VECTOR ( 'NONE', #11112, 1000.000000000000000 ) ;
#18380 = ORIENTED_EDGE ( 'NONE', *, *, #10459, .T. ) ;
#18381 = ORIENTED_EDGE ( 'NONE', *, *, #23008, .F. ) ;
#18382 = VERTEX_POINT ( 'NONE', #16236 ) ;
#18383 = DIRECTION ( 'NONE',  ( 2.257749542879999954E-12, 0.000000000000000000, 1.000000000000000000 ) ) ;
#18384 = CARTESIAN_POINT ( 'NONE',  ( 13.13369214859999978, 51.50000000000000000, -136.5552959530000123 ) ) ;
#18385 = EDGE_CURVE ( 'NONE', #16693, #4825, #23489, .T. ) ;
#18386 = DIRECTION ( 'NONE',  ( 2.257157423930000049E-12, 0.000000000000000000, 1.000000000000000000 ) ) ;
#18387 = VERTEX_POINT ( 'NONE', #18135 ) ;
#18388 = CARTESIAN_POINT ( 'NONE',  ( 24.90181682663759943, 34.66060904161630418, -136.0552959530562021 ) ) ;
#18389 = CARTESIAN_POINT ( 'NONE',  ( -20.51299658253075009, 36.06115981397903170, -140.1078951487501456 ) ) ;
#18390 = CARTESIAN_POINT ( 'NONE',  ( 8.750000000000000000, -42.23606797749999942, -150.0552959529999839 ) ) ;
#18391 = ORIENTED_EDGE ( 'NONE', *, *, #7638, .T. ) ;
#18392 = CARTESIAN_POINT ( 'NONE',  ( -19.89304997513555051, 37.75112169002715490, -140.6578993746063020 ) ) ;
#18393 = VECTOR ( 'NONE', #20645, 1000.000000000000000 ) ;
#18394 = EDGE_CURVE ( 'NONE', #16983, #18478, #1849, .T. ) ;
#18395 = CARTESIAN_POINT ( 'NONE',  ( 9.914807690894544834, 37.49948418880605772, -141.6055286361879553 ) ) ;
#18396 = CARTESIAN_POINT ( 'NONE',  ( -17.91974642297901354, 36.92811127467708587, -148.3783205066631297 ) ) ;
#18397 = CARTESIAN_POINT ( 'NONE',  ( 18.95053822279999878, 50.00000000000000000, -151.0552959529999839 ) ) ;
#18398 = ORIENTED_EDGE ( 'NONE', *, *, #11820, .F. ) ;
#18399 = ADVANCED_FACE ( 'NONE', ( #2317 ), #22173, .F. ) ;
#18400 = EDGE_CURVE ( 'NONE', #3916, #1162, #20735, .T. ) ;
#18401 = DIRECTION ( 'NONE',  ( -2.602084704489999637E-17, 1.000000000000000000, 0.000000000000000000 ) ) ;
#18402 = ORIENTED_EDGE ( 'NONE', *, *, #16197, .F. ) ;
#18403 = LINE ( 'NONE', #2113, #15518 ) ;
#18404 = ADVANCED_FACE ( 'NONE', ( #15269 ), #10862, .F. ) ;
#18405 = ORIENTED_EDGE ( 'NONE', *, *, #5639, .F. ) ;
#18406 = CARTESIAN_POINT ( 'NONE',  ( -26.39256767726975994, 41.50003988705911695, -143.5805134116048123 ) ) ;
#18407 = ORIENTED_EDGE ( 'NONE', *, *, #18623, .T. ) ;
#18408 = VECTOR ( 'NONE', #5878, 1000.000000000000000 ) ;
#18409 = CARTESIAN_POINT ( 'NONE',  ( -2.499999999969999998, 34.00000000000000000, -136.5552959530000123 ) ) ;
#18410 = ADVANCED_FACE ( 'NONE', ( #20479 ), #7502, .F. ) ;
#18411 = EDGE_LOOP ( 'NONE', ( #22880, #12191 ) ) ;
#18412 = PLANE ( 'NONE',  #9431 ) ;
#18413 = VERTEX_POINT ( 'NONE', #15000 ) ;
#18415 = VERTEX_POINT ( 'NONE', #7844 ) ;
#18414 =( BOUNDED_CURVE ( )  B_SPLINE_CURVE ( 5, ( #10630, #535, #18268, #16472, #7767, #10987 ),
 .UNSPECIFIED., .F., .F. ) 
 B_SPLINE_CURVE_WITH_KNOTS ( ( 6, 6 ),
 ( 0.000000000000000000, 1.570796326821625399 ),
 .UNSPECIFIED. ) 
 CURVE ( )  GEOMETRIC_REPRESENTATION_ITEM ( )  RATIONAL_B_SPLINE_CURVE ( ( 1.000000000000000000, 0.5999999999932199568, 0.3999999999932200012, 0.2999999999949150009, 0.2499999999966100173, 0.2500000000000000000 ) ) 
 REPRESENTATION_ITEM ( '' )  );
#18416 = LINE ( 'NONE', #569, #5316 ) ;
#18417 = CARTESIAN_POINT ( 'NONE',  ( -7.305231917150000420, 34.61982510829999882, -147.5275646999999992 ) ) ;
#18418 = CARTESIAN_POINT ( 'NONE',  ( 13.00952979661476583, 24.25756286942641538, -150.0552959529999839 ) ) ;
#18419 = DIRECTION ( 'NONE',  ( 1.000000000000000000, 0.000000000000000000, 0.000000000000000000 ) ) ;
#18420 = CARTESIAN_POINT ( 'NONE',  ( -11.38486064716495960, 36.95668670071903961, -140.3965526140712257 ) ) ;
#18421 = CARTESIAN_POINT ( 'NONE',  ( -8.814413626191640816, 41.18437930593979956, -141.5628561694050234 ) ) ;
#18422 = EDGE_LOOP ( 'NONE', ( #10672, #12692, #2611, #1098 ) ) ;
#18423 = CYLINDRICAL_SURFACE ( 'NONE', #10566, 7.000000000000000888 ) ;
#18424 = DIRECTION ( 'NONE',  ( 1.000000000000000000, 0.000000000000000000, 0.000000000000000000 ) ) ;
#18425 = CIRCLE ( 'NONE', #14250, 2.000000000000000000 ) ;
#18426 = EDGE_LOOP ( 'NONE', ( #4475, #1677, #22375, #4455 ) ) ;
#18427 = LINE ( 'NONE', #7705, #18503 ) ;
#18428 = CARTESIAN_POINT ( 'NONE',  ( -11.68420994714742100, 39.25205177013263125, -141.0178453346331935 ) ) ;
#18429 = EDGE_CURVE ( 'NONE', #12791, #11661, #501, .T. ) ;
#18430 = FACE_OUTER_BOUND ( 'NONE', #5433, .T. ) ;
#18431 = CARTESIAN_POINT ( 'NONE',  ( -29.94412816112640030, 41.23953273985599566, -145.7122098474877987 ) ) ;
#18432 = EDGE_LOOP ( 'NONE', ( #22830, #15285, #1047, #1873 ) ) ;
#18433 = CARTESIAN_POINT ( 'NONE',  ( -7.427142538590000065, 36.18616221519999954, -139.9783837409999876 ) ) ;
#18434 = CARTESIAN_POINT ( 'NONE',  ( -36.62235836789999865, 14.00000000000000000, -143.5552959529999839 ) ) ;
#18435 = ORIENTED_EDGE ( 'NONE', *, *, #3502, .T. ) ;
#18436 = DIRECTION ( 'NONE',  ( 0.1000233216789610108, 0.9949850929136109245, -3.588240815588595806E-13 ) ) ;
#18437 = CARTESIAN_POINT ( 'NONE',  ( -17.42663577349999926, 38.80963643279999786, -139.8270276149999916 ) ) ;
#18438 = PLANE ( 'NONE',  #12859 ) ;
#18439 = CARTESIAN_POINT ( 'NONE',  ( -19.86433599696554353, 39.82348905163189556, -140.3451089131285698 ) ) ;
#18440 = EDGE_LOOP ( 'NONE', ( #10540, #3131, #1307, #18793 ) ) ;
#18441 = CARTESIAN_POINT ( 'NONE',  ( -27.95514704228551750, 33.86422026307950262, -145.8098529824889340 ) ) ;
#18442 = DIRECTION ( 'NONE',  ( 0.7071067811866730279, 0.3390050494208429743, 0.6205445805637129775 ) ) ;
#18443 = LINE ( 'NONE', #11282, #21633 ) ;
#18444 = VECTOR ( 'NONE', #19407, 1000.000000000000000 ) ;
#18445 = LINE ( 'NONE', #17004, #11853 ) ;
#18446 = CARTESIAN_POINT ( 'NONE',  ( -11.19828263940000035, 35.50589712219999683, -140.5907466439999780 ) ) ;
#18447 = ORIENTED_EDGE ( 'NONE', *, *, #978, .F. ) ;
#18448 = LINE ( 'NONE', #13200, #5649 ) ;
#18449 = PLANE ( 'NONE',  #11316 ) ;
#18450 = ORIENTED_EDGE ( 'NONE', *, *, #22462, .T. ) ;
#18451 = VERTEX_POINT ( 'NONE', #14766 ) ;
#18452 =( BOUNDED_CURVE ( )  B_SPLINE_CURVE ( 5, ( #20864, #13717, #2545, #13591, #11921, #7994 ),
 .UNSPECIFIED., .F., .F. ) 
 B_SPLINE_CURVE_WITH_KNOTS ( ( 6, 6 ),
 ( 0.000000000000000000, 1.570796326769926088 ),
 .UNSPECIFIED. ) 
 CURVE ( )  GEOMETRIC_REPRESENTATION_ITEM ( )  RATIONAL_B_SPLINE_CURVE ( ( 1.000000000000000000, 0.6000000000063849814, 0.4000000000063849703, 0.3000000000047887139, 0.2500000000031924463, 0.2499999999999999445 ) ) 
 REPRESENTATION_ITEM ( '' )  );
#18453 = DIRECTION ( 'NONE',  ( -0.06298685227120542907, -0.9980143568310855251, 1.515824502950130739E-13 ) ) ;
#18454 = ADVANCED_FACE ( 'NONE', ( #4298 ), #14889, .T. ) ;
#18455 = DIRECTION ( 'NONE',  ( 1.527666881879999979E-13, 8.171241461240000022E-13, 1.000000000000000000 ) ) ;
#18456 = CARTESIAN_POINT ( 'NONE',  ( -21.53618355989999955, 33.35162261420000362, -146.0341402270000231 ) ) ;
#18457 = CARTESIAN_POINT ( 'NONE',  ( 7.350211351706771090, 36.03637995787053683, -141.7484567678159806 ) ) ;
#18458 = AXIS2_PLACEMENT_3D ( 'NONE', #6167, #20685, #11618 ) ;
#18459 = EDGE_LOOP ( 'NONE', ( #540, #6374 ) ) ;
#18460 = DIRECTION ( 'NONE',  ( 0.000000000000000000, 1.000000000000000000, 0.000000000000000000 ) ) ;
#18461 = VECTOR ( 'NONE', #18262, 1000.000000000000000 ) ;
#18462 = CARTESIAN_POINT ( 'NONE',  ( -19.48816230402476180, 36.23023348068691973, -140.2952556285365802 ) ) ;
#18463 = PLANE ( 'NONE',  #18532 ) ;
#18464 = DIRECTION ( 'NONE',  ( 1.000000000000000000, 0.000000000000000000, 2.516505522483685870E-12 ) ) ;
#18465 = CARTESIAN_POINT ( 'NONE',  ( -23.24304760862829156, 39.89470199026986563, -140.1709173790817999 ) ) ;
#18466 = CARTESIAN_POINT ( 'NONE',  ( -15.57786843150000067, 37.00666880280000726, -148.5521201120000114 ) ) ;
#18467 = CARTESIAN_POINT ( 'NONE',  ( -34.50000000000000000, 76.00000000000000000, -132.5552959530000123 ) ) ;
#18468 = LINE ( 'NONE', #4073, #6534 ) ;
#18469 = LINE ( 'NONE', #16683, #3960 ) ;
#18470 = ORIENTED_EDGE ( 'NONE', *, *, #13374, .T. ) ;
#18471 = CARTESIAN_POINT ( 'NONE',  ( -5.764515702665429231, 39.05871236480190589, -141.1073062976952599 ) ) ;
#18472 = CIRCLE ( 'NONE', #13921, 2.500000000000002220 ) ;
#18473 = AXIS2_PLACEMENT_3D ( 'NONE', #17879, #23113, #14187 ) ;
#18474 = EDGE_LOOP ( 'NONE', ( #11109, #11197, #2206, #7800 ) ) ;
#18475 = CARTESIAN_POINT ( 'NONE',  ( 7.500000000000000000, -3.500000000000000000, -140.0552959529999839 ) ) ;
#18476 = CARTESIAN_POINT ( 'NONE',  ( -22.82643395159999855, 32.86988923359999859, -143.6006525860000238 ) ) ;
#18477 = FACE_OUTER_BOUND ( 'NONE', #3695, .T. ) ;
#18478 = VERTEX_POINT ( 'NONE', #11526 ) ;
#18479 = CARTESIAN_POINT ( 'NONE',  ( -13.52923207339164335, 35.54581745406167670, -140.8134052129221061 ) ) ;
#18480 = EDGE_CURVE ( 'NONE', #1486, #21613, #19632, .T. ) ;
#18481 = LINE ( 'NONE', #5283, #6680 ) ;
#18482 = CARTESIAN_POINT ( 'NONE',  ( 12.57628698940784773, 35.71923945895441221, -150.0552959529999839 ) ) ;
#18483 = DIRECTION ( 'NONE',  ( 1.000000000000000000, 0.000000000000000000, -2.253752739989067373E-12 ) ) ;
#18484 = EDGE_CURVE ( 'NONE', #13874, #22942, #16786, .T. ) ;
#18485 = CARTESIAN_POINT ( 'NONE',  ( -32.50000000000000000, -51.50000000000000000, -137.0552959530000123 ) ) ;
#18486 = PLANE ( 'NONE',  #1466 ) ;
#18487 = ORIENTED_EDGE ( 'NONE', *, *, #17167, .F. ) ;
#18488 = AXIS2_PLACEMENT_3D ( 'NONE', #2923, #13748, #21012 ) ;
#18489 = LINE ( 'NONE', #20639, #13648 ) ;
#18490 = VERTEX_POINT ( 'NONE', #3947 ) ;
#18491 = ORIENTED_EDGE ( 'NONE', *, *, #17380, .F. ) ;
#18492 = LINE ( 'NONE', #8970, #6906 ) ;
#18493 = CARTESIAN_POINT ( 'NONE',  ( -9.834719431799998191, 32.58365614919999587, -144.2353630830000100 ) ) ;
#18494 = CARTESIAN_POINT ( 'NONE',  ( 11.45511797039051061, 26.15112731430704684, -136.0552959530258761 ) ) ;
#18495 = EDGE_LOOP ( 'NONE', ( #4542, #6727, #9742, #18774, #1191, #884, #13042, #7466, #18014, #9381, #2911, #13903 ) ) ;
#18496 = DIRECTION ( 'NONE',  ( 0.000000000000000000, 0.000000000000000000, -1.000000000000000000 ) ) ;
#18497 = PLANE ( 'NONE',  #16344 ) ;
#18498 = CYLINDRICAL_SURFACE ( 'NONE', #7156, 1.500000000000000444 ) ;
#18499 = ORIENTED_EDGE ( 'NONE', *, *, #9951, .T. ) ;
#18500 = CARTESIAN_POINT ( 'NONE',  ( -21.44245888780737630, 40.16992768860739460, -145.8848771850359469 ) ) ;
#18501 = VECTOR ( 'NONE', #19075, 1000.000000000000000 ) ;
#18502 = CARTESIAN_POINT ( 'NONE',  ( 9.864092401084887385, 37.62553476576535161, -141.6344350118990576 ) ) ;
#18503 = VECTOR ( 'NONE', #468, 1000.000000000000000 ) ;
#18504 = CARTESIAN_POINT ( 'NONE',  ( 31.50000000000000000, 40.03620104880000241, -136.0552959530000123 ) ) ;
#18505 = CARTESIAN_POINT ( 'NONE',  ( -21.71608528419999828, -1.500000000000000000, -144.8157682190000060 ) ) ;
#18506 = ORIENTED_EDGE ( 'NONE', *, *, #9657, .F. ) ;
#18507 = DIRECTION ( 'NONE',  ( 0.6459422414661299960, 0.7633862853691516515, 0.000000000000000000 ) ) ;
#18508 = ORIENTED_EDGE ( 'NONE', *, *, #19567, .F. ) ;
#18510 = ORIENTED_EDGE ( 'NONE', *, *, #16151, .F. ) ;
#18509 = VECTOR ( 'NONE', #5417, 1000.000000000000000 ) ;
#18511 = CARTESIAN_POINT ( 'NONE',  ( -26.61767157499349423, 39.52029466085011222, -147.6008517105564408 ) ) ;
#18512 = ORIENTED_EDGE ( 'NONE', *, *, #17707, .T. ) ;
#18513 = CARTESIAN_POINT ( 'NONE',  ( -22.03156944974935882, 33.39557638551315932, -141.8445571067651940 ) ) ;
#18514 = ADVANCED_FACE ( 'NONE', ( #18804 ), #9626, .F. ) ;
#18515 = VECTOR ( 'NONE', #3513, 1000.000000000000000 ) ;
#18516 = ORIENTED_EDGE ( 'NONE', *, *, #6416, .T. ) ;
#18517 = DIRECTION ( 'NONE',  ( 0.000000000000000000, 0.000000000000000000, 1.000000000000000000 ) ) ;
#18518 = ORIENTED_EDGE ( 'NONE', *, *, #22617, .T. ) ;
#18519 = DIRECTION ( 'NONE',  ( 0.9338042224025928650, -0.3577843962822991886, -2.107731196709189395E-12 ) ) ;
#18520 = ORIENTED_EDGE ( 'NONE', *, *, #11777, .F. ) ;
#18521 = CARTESIAN_POINT ( 'NONE',  ( -28.00347998519043458, 37.05747243973696925, -148.5422211677327766 ) ) ;
#18522 = DIRECTION ( 'NONE',  ( -2.257144641399999941E-12, 0.000000000000000000, -1.000000000000000000 ) ) ;
#18523 = DIRECTION ( 'NONE',  ( 1.000000000000000000, 0.000000000000000000, -1.498801083243961330E-13 ) ) ;
#18524 = DIRECTION ( 'NONE',  ( -2.842170943040000002E-14, -3.570477247189999985E-13, -1.000000000000000000 ) ) ;
#18525 = CARTESIAN_POINT ( 'NONE',  ( -6.166004029541136688, 36.95750611116264395, -148.6250205690584210 ) ) ;
#18526 = EDGE_CURVE ( 'NONE', #13267, #683, #11947, .T. ) ;
#18527 = DIRECTION ( 'NONE',  ( 1.000000000000000000, 0.000000000000000000, 0.000000000000000000 ) ) ;
#18528 = ORIENTED_EDGE ( 'NONE', *, *, #19104, .F. ) ;
#18529 = EDGE_CURVE ( 'NONE', #18413, #23072, #3832, .T. ) ;
#18530 = DIRECTION ( 'NONE',  ( 0.000000000000000000, 0.000000000000000000, 1.000000000000000000 ) ) ;
#18531 = EDGE_CURVE ( 'NONE', #13091, #21066, #5722, .T. ) ;
#18532 = AXIS2_PLACEMENT_3D ( 'NONE', #13099, #4190, #11424 ) ;
#18533 = DIRECTION ( 'NONE',  ( -0.9892101392001054760, 0.1465035852930155480, 4.471739159800472250E-12 ) ) ;
#18534 = EDGE_CURVE ( 'NONE', #3203, #18084, #15243, .T. ) ;
#18535 = CIRCLE ( 'NONE', #8264, 0.5000000000000004441 ) ;
#18536 = ORIENTED_EDGE ( 'NONE', *, *, #3868, .T. ) ;
#18537 = LINE ( 'NONE', #9920, #8602 ) ;
#18538 = CARTESIAN_POINT ( 'NONE',  ( -12.84574840978007693, 37.96884797463420114, -148.5681481162234263 ) ) ;
#18539 = PLANE ( 'NONE',  #15479 ) ;
#18540 = CARTESIAN_POINT ( 'NONE',  ( -29.55850978561355902, 41.47329217818079883, -142.4456950392344083 ) ) ;
#18541 = ORIENTED_EDGE ( 'NONE', *, *, #4351, .F. ) ;
#18542 = DIRECTION ( 'NONE',  ( 0.000000000000000000, -1.000000000000000000, 0.000000000000000000 ) ) ;
#18543 = CARTESIAN_POINT ( 'NONE',  ( -21.35824191589999899, -32.75000000000000000, -145.5657682190000060 ) ) ;
#18544 = ORIENTED_EDGE ( 'NONE', *, *, #17082, .F. ) ;
#18545 = LINE ( 'NONE', #241, #17076 ) ;
#18546 = DIRECTION ( 'NONE',  ( -1.527666881879999979E-13, -8.171241461240000022E-13, -1.000000000000000000 ) ) ;
#18547 = EDGE_LOOP ( 'NONE', ( #4029, #21921, #11152, #10705 ) ) ;
#18548 = FACE_OUTER_BOUND ( 'NONE', #22339, .T. ) ;
#18549 = EDGE_CURVE ( 'NONE', #20660, #3881, #8965, .T. ) ;
#18550 = CARTESIAN_POINT ( 'NONE',  ( -20.68104909725491680, 41.14100626298056085, -146.5604280120006990 ) ) ;
#18551 = EDGE_LOOP ( 'NONE', ( #9423, #5926, #9703, #21881, #18911, #20034, #2491, #4472, #8578, #499, #3563 ) ) ;
#18552 =( NAMED_UNIT ( * ) SI_UNIT ( $, .STERADIAN. ) SOLID_ANGLE_UNIT ( ) );
#18553 = CARTESIAN_POINT ( 'NONE',  ( -24.00000000000000000, 47.50000000000000000, -151.0552959529999839 ) ) ;
#18554 = AXIS2_PLACEMENT_3D ( 'NONE', #12239, #2978, #19034 ) ;
#18555 = DIRECTION ( 'NONE',  ( -0.1435602414469281940, -0.9896415801065048257, 3.836930773098079160E-13 ) ) ;
#18556 = ORIENTED_EDGE ( 'NONE', *, *, #1419, .F. ) ;
#18557 = LINE ( 'NONE', #4391, #15532 ) ;
#18558 = AXIS2_PLACEMENT_3D ( 'NONE', #3301, #10537, #17820 ) ;
#18559 = CARTESIAN_POINT ( 'NONE',  ( 1.713198289069999936, -17.44292009260000142, -147.5552959529999839 ) ) ;
#18560 = FACE_OUTER_BOUND ( 'NONE', #14564, .T. ) ;
#18561 = ORIENTED_EDGE ( 'NONE', *, *, #14325, .T. ) ;
#18562 = EDGE_CURVE ( 'NONE', #17085, #17118, #21191, .T. ) ;
#18563 = DIRECTION ( 'NONE',  ( -1.000000000000000000, 5.094701932209999624E-24, 0.000000000000000000 ) ) ;
#18564 = EDGE_CURVE ( 'NONE', #8517, #18121, #17489, .T. ) ;
#18565 = LINE ( 'NONE', #9507, #10946 ) ;
#18566 = ORIENTED_EDGE ( 'NONE', *, *, #4121, .T. ) ;
#18567 = EDGE_CURVE ( 'NONE', #13091, #12006, #7079, .T. ) ;
#18568 = ORIENTED_EDGE ( 'NONE', *, *, #6601, .F. ) ;
#18569 = CARTESIAN_POINT ( 'NONE',  ( -23.31991597950000283, 35.31558869410000057, -140.3324749399999973 ) ) ;
#18570 = VECTOR ( 'NONE', #3183, 1000.000000000000000 ) ;
#18571 = CARTESIAN_POINT ( 'NONE',  ( -30.41918043656675508, 40.92081927820395748, -146.2642377558170494 ) ) ;
#18572 = CYLINDRICAL_SURFACE ( 'NONE', #8246, 0.5000000000000079936 ) ;
#18573 = CARTESIAN_POINT ( 'NONE',  ( 7.625014772252407091, 35.78154871851074148, -141.8721224017280917 ) ) ;
#18574 = VERTEX_POINT ( 'NONE', #22722 ) ;
#18575 = SURFACE_SIDE_STYLE ('',( #4064 ) ) ;
#18576 = CARTESIAN_POINT ( 'NONE',  ( 24.36715301250000110, -30.57462384669999977, -147.5552959529999839 ) ) ;
#18577 = AXIS2_PLACEMENT_3D ( 'NONE', #10512, #1634, #10403 ) ;
#18578 = DIRECTION ( 'NONE',  ( 0.6459422414661314393, -0.7633862853691505412, 0.000000000000000000 ) ) ;
#18579 = DIRECTION ( 'NONE',  ( 1.000000000000000000, 0.000000000000000000, -1.701177084980000217E-20 ) ) ;
#18580 = VECTOR ( 'NONE', #1077, 1000.000000000000227 ) ;
#18581 = CARTESIAN_POINT ( 'NONE',  ( -23.86695900996863884, 38.68196870774303164, -148.0474502902359859 ) ) ;
#18582 = CARTESIAN_POINT ( 'NONE',  ( -15.57778390732538298, 34.09428877113495560, -147.7625705869996580 ) ) ;
#18583 = ADVANCED_BREP_SHAPE_REPRESENTATION ( '', ( #19475, #5025 ), #19488 ) ;
#18584 = CARTESIAN_POINT ( 'NONE',  ( -19.36113520410000177, 33.15198947340000046, -146.5298456060000092 ) ) ;
#18585 = DIRECTION ( 'NONE',  ( 0.000000000000000000, 1.592654863519999645E-17, -1.000000000000000000 ) ) ;
#18586 = CARTESIAN_POINT ( 'NONE',  ( -22.10824191591069265, -4.000000000000000000, -141.9623572383543717 ) ) ;
#18587 = CIRCLE ( 'NONE', #17845, 6.000000000000001776 ) ;
#18588 = ORIENTED_EDGE ( 'NONE', *, *, #21321, .T. ) ;
#18589 = EDGE_CURVE ( 'NONE', #1386, #13765, #19400, .T. ) ;
#18590 = CARTESIAN_POINT ( 'NONE',  ( -5.972224716156503632, 40.79464204724823873, -141.7656025440403766 ) ) ;
#18591 = DIRECTION ( 'NONE',  ( -0.9938526945756316344, 0.1107105301439589573, 6.178155812097707047E-14 ) ) ;
#18592 = VECTOR ( 'NONE', #19658, 1000.000000000000000 ) ;
#18593 = ADVANCED_FACE ( 'NONE', ( #19039 ), #22501, .T. ) ;
#18594 = EDGE_LOOP ( 'NONE', ( #2585, #17437, #21133 ) ) ;
#18595 = CIRCLE ( 'NONE', #11351, 5.000000000000000000 ) ;
#18596 =( LENGTH_UNIT ( ) NAMED_UNIT ( * ) SI_UNIT ( .MILLI., .METRE. ) );
#18597 = AXIS2_PLACEMENT_3D ( 'NONE', #22934, #2937, #2710 ) ;
#18598 = CIRCLE ( 'NONE', #10229, 1.500000000000001332 ) ;
#18599 = CARTESIAN_POINT ( 'NONE',  ( -22.23138069775068004, 34.62558912611336126, -140.6296127981910047 ) ) ;
#18600 = DIRECTION ( 'NONE',  ( 1.211690350419999855E-27, 2.765629237170000203E-27, -1.000000000000000000 ) ) ;
#18601 = ORIENTED_EDGE ( 'NONE', *, *, #3436, .F. ) ;
#18602 = CARTESIAN_POINT ( 'NONE',  ( -12.47706116150000000, 35.17890886639999337, -148.2557368829999973 ) ) ;
#18603 = FACE_OUTER_BOUND ( 'NONE', #4495, .T. ) ;
#18604 = CARTESIAN_POINT ( 'NONE',  ( 13.66060904159877154, 34.09818317339773586, -150.0552959529999839 ) ) ;
#18605 = DIRECTION ( 'NONE',  ( -0.1146332952500066227, -0.9934078757590583120, -9.947598300640582187E-14 ) ) ;
#18606 = DIRECTION ( 'NONE',  ( -1.457881434619999915E-12, -1.723066134219999902E-12, 1.000000000000000000 ) ) ;
#18607 = VECTOR ( 'NONE', #10059, 1000.000000000000000 ) ;
#18608 = CARTESIAN_POINT ( 'NONE',  ( 3.906463970568107236, -37.00246044238615184, -150.0552959529999839 ) ) ;
#18609 = VERTEX_POINT ( 'NONE', #20955 ) ;
#18610 = VECTOR ( 'NONE', #455, 1000.000000000000000 ) ;
#18611 = VECTOR ( 'NONE', #4453, 1000.000000000000000 ) ;
#18612 = CARTESIAN_POINT ( 'NONE',  ( -28.48845118146442346, 34.53992523626719446, -147.5004638035997573 ) ) ;
#18613 = ORIENTED_EDGE ( 'NONE', *, *, #21600, .F. ) ;
#18614 =( NAMED_UNIT ( * ) SI_UNIT ( $, .STERADIAN. ) SOLID_ANGLE_UNIT ( ) );
#18615 = AXIS2_PLACEMENT_3D ( 'NONE', #3221, #7018, #10345 ) ;
#18616 = VECTOR ( 'NONE', #8304, 1000.000000000000000 ) ;
#18617 = ORIENTED_EDGE ( 'NONE', *, *, #12858, .F. ) ;
#18618 = CARTESIAN_POINT ( 'NONE',  ( -14.30645844936410427, 35.39002938633848316, -140.6974358100255529 ) ) ;
#18619 = DIRECTION ( 'NONE',  ( -1.000000000000000000, -2.808280234649999694E-18, -2.507771768019999718E-12 ) ) ;
#18620 = CARTESIAN_POINT ( 'NONE',  ( -31.00000000000000000, -7.105427357599999217E-15, -149.5552959529999839 ) ) ;
#18621 = EDGE_CURVE ( 'NONE', #7036, #12734, #2862, .T. ) ;
#18622 = EDGE_LOOP ( 'NONE', ( #9234, #7256, #7325, #13008 ) ) ;
#18623 = EDGE_CURVE ( 'NONE', #11516, #5773, #6541, .T. ) ;
#18624 = LINE ( 'NONE', #13028, #14829 ) ;
#18625 = CARTESIAN_POINT ( 'NONE',  ( 11.68320006079999906, -20.50000000000000000, -150.0552959529999839 ) ) ;
#18626 = ADVANCED_FACE ( 'NONE', ( #6652 ), #22854, .F. ) ;
#18627 = ORIENTED_EDGE ( 'NONE', *, *, #1285, .T. ) ;
#18628 = CARTESIAN_POINT ( 'NONE',  ( 14.00000000004000356, 19.51825229575318588, -136.0552959530169517 ) ) ;
#18629 = CARTESIAN_POINT ( 'NONE',  ( 9.033660455730478489, 38.40283821535013686, -141.9858703027461786 ) ) ;
#18630 = AXIS2_PLACEMENT_3D ( 'NONE', #1753, #19831, #10759 ) ;
#18631 = AXIS2_PLACEMENT_3D ( 'NONE', #13853, #22658, #6589 ) ;
#18632 = DIRECTION ( 'NONE',  ( -8.955503005839999404E-12, 9.112710586119999183E-13, -1.000000000000000000 ) ) ;
#18633 = PLANE ( 'NONE',  #13952 ) ;
#18634 = ORIENTED_EDGE ( 'NONE', *, *, #7700, .F. ) ;
#18635 = DIRECTION ( 'NONE',  ( 0.000000000000000000, 1.000000000000000000, 0.000000000000000000 ) ) ;
#18636 = ORIENTED_EDGE ( 'NONE', *, *, #17652, .F. ) ;
#18637 = LINE ( 'NONE', #9576, #10167 ) ;
#18638 = ORIENTED_EDGE ( 'NONE', *, *, #10917, .F. ) ;
#18639 = CARTESIAN_POINT ( 'NONE',  ( -27.06022691664431790, 38.83733237976459662, -148.2479545113073982 ) ) ;
#18640 = VERTEX_POINT ( 'NONE', #12007 ) ;
#18641 = CARTESIAN_POINT ( 'NONE',  ( -22.82187525211859125, 36.04812013258515435, -139.3733050199115837 ) ) ;
#18642 = ORIENTED_EDGE ( 'NONE', *, *, #15487, .F. ) ;
#18643 = FACE_OUTER_BOUND ( 'NONE', #3669, .T. ) ;
#18644 = ORIENTED_EDGE ( 'NONE', *, *, #20195, .F. ) ;
#18645 = DIRECTION ( 'NONE',  ( 1.000000000000000000, 0.000000000000000000, 0.000000000000000000 ) ) ;
#18646 = CIRCLE ( 'NONE', #6095, 5.000000000000000000 ) ;
#18647 = VECTOR ( 'NONE', #4456, 1000.000000000000000 ) ;
#18648 = ORIENTED_EDGE ( 'NONE', *, *, #13640, .T. ) ;
#18649 = DIRECTION ( 'NONE',  ( -2.508215857230000030E-12, 0.000000000000000000, 1.000000000000000000 ) ) ;
#18650 = FACE_OUTER_BOUND ( 'NONE', #18432, .T. ) ;
#18651 = CARTESIAN_POINT ( 'NONE',  ( 6.992624432235133192, 28.00000000000000711, -150.0552959530000408 ) ) ;
#18652 = EDGE_CURVE ( 'NONE', #12670, #6404, #19934, .T. ) ;
#18653 = DIRECTION ( 'NONE',  ( -1.000000000000000000, 1.458293570536846221E-24, 2.257144641401985094E-12 ) ) ;
#18654 = DIRECTION ( 'NONE',  ( -0.6459422414661292189, 0.7633862853691524286, 0.000000000000000000 ) ) ;
#18655 = CARTESIAN_POINT ( 'NONE',  ( -8.170418261672836024, 39.82841872393940008, -140.1620592250056347 ) ) ;
#18656 = ORIENTED_EDGE ( 'NONE', *, *, #12222, .F. ) ;
#18657 = CARTESIAN_POINT ( 'NONE',  ( -32.50000000000000000, 26.00000000000000000, -137.5552959530000123 ) ) ;
#18658 = B_SPLINE_CURVE_WITH_KNOTS ( 'NONE', 3,
 ( #17403, #1124, #22892, #6575, #21104, #19308, #8471, #22998, #15738, #6688, #21574, #23464, #7040, #3480, #14303, #21815, #1823, #23351, #10718, #8693, #1709, #10477, #21697, #21341, #12632, #3242, #17999, #5499, #8929, #6807, #8577, #12745, #12507, #16212, #1597, #14426, #19903, #15974, #14074, #3713, #16094, #3356, #23116, #5383, #10595, #38, #20018, #3602, #17643, #5256, #19788, #5034, #17881, #7160, #12386, #14551, #6929, #10828, #12275, #17753, #1351, #18113, #19549, #19661, #9042, #16331, #7282, #15849, #1471, #23234, #14190, #21455, #5135, #8818, #15003, #18457, #20602, #614, #11297, #20366, #7622, #4062, #14892, #15118, #18701, #16669, #18573, #2061, #2297, #7848, #383, #7505, #5839, #9518, #16903, #22153, #13095, #10951, #16791, #2412, #5725, #504, #2172, #7737, #13209, #9282, #153, #18236, #9393, #22264, #22040, #5954 ),
 .UNSPECIFIED., .F., .F.,
 ( 4, 2, 1, 2, 2, 2, 1, 1, 2, 2, 2, 2, 1, 1, 1, 2, 2, 2, 2, 2, 1, 2, 2, 2, 2, 1, 2, 2, 2, 1, 2, 2, 2, 2, 2, 1, 2, 2, 2, 1, 1, 2, 2, 2, 2, 1, 1, 2, 2, 2, 2, 1, 1, 1, 2, 2, 2, 1, 1, 2, 2, 2, 1, 2, 2, 4 ),
 ( 0.000000000000000000, 0.03124999999964979402, 0.04687499999947458001, 0.05468749999938697648, 0.06249999999929936600, 0.09374999999895526626, 0.1093749999987843197, 0.1171874999986995819, 0.1210937499986559779, 0.1249999999986123878, 0.1562499999982641941, 0.1718749999980896670, 0.1796874999980059007, 0.1835937499979638510, 0.1855468749979440057, 0.1865234374979332643, 0.1874999999979225507, 0.2187499999978837206, 0.2343749999978601839, 0.2421874999978483878, 0.2460937499978433918, 0.2480468749978424203, 0.2499999999978414489, 0.2812499999978634313, 0.2968749999978704257, 0.3046874999978750886, 0.3085937499978803067, 0.3124999999978855247, 0.3437499999979258813, 0.3593749999979464760, 0.3671874999979566345, 0.3749999999979667931, 0.4999999999981064036, 0.5624999999981761256, 0.5937499999982130960, 0.6093749999982316368, 0.6171874999982408516, 0.6249999999982500665, 0.6562499999982865928, 0.6718749999983006926, 0.6796874999983039123, 0.6835937499983055776, 0.6874999999983072430, 0.7187499999982993604, 0.7343749999982969179, 0.7421874999982993604, 0.7460937499982994714, 0.7480468749983008037, 0.7499999999983021359, 0.7812499999983306687, 0.7968749999983447685, 0.8046874999983562038, 0.8085937499983619769, 0.8105468749983758547, 0.8115234374983829602, 0.8124999999983899546, 0.8437499999986364241, 0.8593749999987574384, 0.8671874999988179455, 0.8710937499988491428, 0.8749999999988802291, 0.9062499999991531219, 0.9218749999992918998, 0.9296874999993632871, 0.9374999999994347855, 1.000000000000000000 ),
 .UNSPECIFIED. ) ;
#18659 = PRODUCT_RELATED_PRODUCT_CATEGORY ( 'part', '', ( #13597 ) ) ;
#18660 = DIRECTION ( 'NONE',  ( 5.094701932209999624E-24, 1.000000000000000000, 0.000000000000000000 ) ) ;
#18661 = ADVANCED_FACE ( 'NONE', ( #4522 ), #17135, .F. ) ;
#18662 = DIRECTION ( 'NONE',  ( 2.507771768019999718E-12, 1.592654864069999939E-17, -1.000000000000000000 ) ) ;
#18663 = VECTOR ( 'NONE', #23408, 1000.000000000000000 ) ;
#18664 = VERTEX_POINT ( 'NONE', #17256 ) ;
#18665 = AXIS2_PLACEMENT_3D ( 'NONE', #18006, #21463, #14433 ) ;
#18666 = CARTESIAN_POINT ( 'NONE',  ( -12.03885416238175132, 41.13341945414818213, -146.5840868153462964 ) ) ;
#18667 = CARTESIAN_POINT ( 'NONE',  ( -17.90603444523116039, 39.81532604249508722, -147.8912533906195961 ) ) ;
#18668 = CARTESIAN_POINT ( 'NONE',  ( -28.82642799346931284, 39.82454263016848017, -141.4161836699787784 ) ) ;
#18669 = VERTEX_POINT ( 'NONE', #6302 ) ;
#18670 = CARTESIAN_POINT ( 'NONE',  ( 1.561837858109999866, -18.84848306830000197, -143.5552959529999839 ) ) ;
#18671 = CARTESIAN_POINT ( 'NONE',  ( -3.500000000000000000, 40.00000000000000000, -150.0552959529999839 ) ) ;
#18672 = ADVANCED_FACE ( 'NONE', ( #13556 ), #11762, .T. ) ;
#18673 = EDGE_LOOP ( 'NONE', ( #17572, #14477, #12311, #7550 ) ) ;
#18674 = LINE ( 'NONE', #2496, #20900 ) ;
#18675 = LINE ( 'NONE', #2387, #16793 ) ;
#18676 = VERTEX_POINT ( 'NONE', #21784 ) ;
#18677 = DIRECTION ( 'NONE',  ( -2.842170943040000002E-14, -3.552713678800000097E-13, -1.000000000000000000 ) ) ;
#18678 = CARTESIAN_POINT ( 'NONE',  ( -20.64937491868320407, 39.51007782554450642, -147.6820107799256050 ) ) ;
#18679 = ORIENTED_EDGE ( 'NONE', *, *, #11430, .T. ) ;
#18680 = SHAPE_REPRESENTATION_RELATIONSHIP ( 'NONE' , 'NONE' ,  #16641, #5808 ) ;
#18681 = CARTESIAN_POINT ( 'NONE',  ( -27.49486172903679204, 36.99676060752978657, -147.4549925864818931 ) ) ;
#18682 = CARTESIAN_POINT ( 'NONE',  ( -11.38486064709999823, 36.95668670079999885, -140.3965526140000009 ) ) ;
#18683 = ORIENTED_EDGE ( 'NONE', *, *, #13457, .F. ) ;
#18684 = DIRECTION ( 'NONE',  ( 1.000000000000000000, 0.000000000000000000, -8.955190032050000935E-12 ) ) ;
#18685 = DIRECTION ( 'NONE',  ( -1.000000000000000000, 0.000000000000000000, 0.000000000000000000 ) ) ;
#18686 = VECTOR ( 'NONE', #22511, 1000.000000000000114 ) ;
#18687 = EDGE_CURVE ( 'NONE', #4104, #1364, #12712, .T. ) ;
#18688 = CARTESIAN_POINT ( 'NONE',  ( -10.47418533549999964, 33.50012463689999720, -145.9259304109999960 ) ) ;
#18689 = VECTOR ( 'NONE', #17571, 1000.000000000000000 ) ;
#18690 = VERTEX_POINT ( 'NONE', #5470 ) ;
#18691 = CARTESIAN_POINT ( 'NONE',  ( 11.29705455228499567, -19.69977967857330725, -148.5552959529999839 ) ) ;
#18692 = CARTESIAN_POINT ( 'NONE',  ( -2.489991676528331865, 46.24652334969331946, -136.0552959529943848 ) ) ;
#18693 = ORIENTED_EDGE ( 'NONE', *, *, #20641, .F. ) ;
#18694 = ADVANCED_FACE ( 'NONE', ( #2 ), #8657, .F. ) ;
#18695 = ADVANCED_FACE ( 'NONE', ( #16179 ), #12471, .T. ) ;
#18696 = ORIENTED_EDGE ( 'NONE', *, *, #3286, .F. ) ;
#18697 = ADVANCED_FACE ( 'NONE', ( #15938 ), #14158, .T. ) ;
#18698 = CARTESIAN_POINT ( 'NONE',  ( 4.500000000009999113, -2.000000000000000000, -136.0552959530000123 ) ) ;
#18699 = CARTESIAN_POINT ( 'NONE',  ( 3.611688725869999975E-11, -50.50000000000000000, -136.0552959530000123 ) ) ;
#18700 = DIRECTION ( 'NONE',  ( -1.000000000000000000, 0.000000000000000000, -2.245315044929999938E-12 ) ) ;
#18701 = CARTESIAN_POINT ( 'NONE',  ( 7.552123853614987503, 35.83646061958899764, -141.8420144836698285 ) ) ;
#18702 = VERTEX_POINT ( 'NONE', #8544 ) ;
#18703 = FILL_AREA_STYLE_COLOUR ( '', #13956 ) ;
#18704 = AXIS2_PLACEMENT_3D ( 'NONE', #6055, #7715, #5931 ) ;
#18705 = CIRCLE ( 'NONE', #15660, 0.7500000000000006661 ) ;
#18706 = CARTESIAN_POINT ( 'NONE',  ( -8.031950161270000166, 40.75709267670000457, -141.9144354160000034 ) ) ;
#18707 = ADVANCED_FACE ( 'NONE', ( #10795 ), #10684, .F. ) ;
#18708 = DIRECTION ( 'NONE',  ( -1.000000000000000000, 0.000000000000000000, -2.507771768020000122E-12 ) ) ;
#18709 = CARTESIAN_POINT ( 'NONE',  ( 16.64676602990000021, -18.64223989710000140, -143.5552959529999839 ) ) ;
#18710 = CARTESIAN_POINT ( 'NONE',  ( -24.28961182125106077, 41.32638505982121302, -143.5933768036660751 ) ) ;
#18711 = EDGE_CURVE ( 'NONE', #15538, #9295, #9012, .T. ) ;
#18712 = CARTESIAN_POINT ( 'NONE',  ( 9.683200060759999062, -20.50000000000000000, -148.5552959529999839 ) ) ;
#18713 = ADVANCED_FACE ( 'NONE', ( #3213 ), #19628, .T. ) ;
#18714 = CARTESIAN_POINT ( 'NONE',  ( -17.43215188622844636, 36.07634741369874831, -139.7482345171883082 ) ) ;
#18715 = EDGE_CURVE ( 'NONE', #10697, #22598, #7009, .T. ) ;
#18716 = CARTESIAN_POINT ( 'NONE',  ( -18.95027878879999861, 36.16636532760000478, -148.4341920939999966 ) ) ;
#18717 = CARTESIAN_POINT ( 'NONE',  ( 15.50000000000000000, 33.50000000000000000, -151.0552959529999839 ) ) ;
#18718 = PLANE ( 'NONE',  #4716 ) ;
#18719 = VERTEX_POINT ( 'NONE', #10337 ) ;
#18720 = CARTESIAN_POINT ( 'NONE',  ( -5.537589236589999686, 40.52957482200000072, -146.1175057039999956 ) ) ;
#18721 = FACE_BOUND ( 'NONE', #21421, .T. ) ;
#18722 = ORIENTED_EDGE ( 'NONE', *, *, #14743, .F. ) ;
#18723 = VECTOR ( 'NONE', #18685, 1000.000000000000000 ) ;
#18724 = CARTESIAN_POINT ( 'NONE',  ( 32.14594224169999848, -40.79958733389999992, -150.0552959529999839 ) ) ;
#18725 = CARTESIAN_POINT ( 'NONE',  ( -21.60271751204859214, 36.29226947926043323, -147.3679125513968131 ) ) ;
#18726 = LINE ( 'NONE', #7869, #11736 ) ;
#18727 = VERTEX_POINT ( 'NONE', #23433 ) ;
#18728 = CARTESIAN_POINT ( 'NONE',  ( -12.76385253889189997, 37.02886902030352445, -147.6186336935166139 ) ) ;
#18729 = DIRECTION ( 'NONE',  ( 0.000000000000000000, 0.000000000000000000, -1.000000000000000000 ) ) ;
#18730 = CARTESIAN_POINT ( 'NONE',  ( -30.50000000000000000, 47.50000000000000000, -149.0552959529999839 ) ) ;
#18731 = CARTESIAN_POINT ( 'NONE',  ( -30.49999999990000177, 37.00000000000000000, -139.0552959529999839 ) ) ;
#18732 = LINE ( 'NONE', #10013, #7791 ) ;
#18733 = CARTESIAN_POINT ( 'NONE',  ( 4.109320143298619499, -4.961756220215326252, -136.0552959530092778 ) ) ;
#18734 = EDGE_LOOP ( 'NONE', ( #23156, #22239, #6320, #2298, #18518, #89, #13703, #11040 ) ) ;
#18735 = EDGE_CURVE ( 'NONE', #18822, #9410, #8781, .T. ) ;
#18736 = FACE_OUTER_BOUND ( 'NONE', #22614, .T. ) ;
#18737 = ORIENTED_EDGE ( 'NONE', *, *, #20103, .T. ) ;
#18738 = CARTESIAN_POINT ( 'NONE',  ( -13.82058007329999860, 36.03909227049999942, -139.5626078809999910 ) ) ;
#18739 = CARTESIAN_POINT ( 'NONE',  ( -9.178237216079999428, 36.01795878010000251, -148.2568923610000127 ) ) ;
#18740 = LINE ( 'NONE', #9781, #16107 ) ;
#18741 = ORIENTED_EDGE ( 'NONE', *, *, #978, .T. ) ;
#18742 = CARTESIAN_POINT ( 'NONE',  ( 8.500000000060001781, 38.50000000000000000, -144.0552959529999839 ) ) ;
#18743 = LINE ( 'NONE', #4454, #10627 ) ;
#18744 = EDGE_LOOP ( 'NONE', ( #4715, #14339, #2847, #15533 ) ) ;
#18745 = DIRECTION ( 'NONE',  ( -0.09606172499277226828, -0.9953753789357124848, 8.268372250837614805E-13 ) ) ;
#18746 = CARTESIAN_POINT ( 'NONE',  ( 9.891652228665913427, 37.55988566378615445, -141.6187646494944659 ) ) ;
#18747 =( GEOMETRIC_REPRESENTATION_CONTEXT ( 3 ) GLOBAL_UNCERTAINTY_ASSIGNED_CONTEXT ( ( #17565 ) ) GLOBAL_UNIT_ASSIGNED_CONTEXT ( ( #2121, #9343, #11139 ) ) REPRESENTATION_CONTEXT ( 'NONE', 'WORKASPACE' ) );
#18748 = FACE_BOUND ( 'NONE', #5307, .T. ) ;
#18749 = CARTESIAN_POINT ( 'NONE',  ( -25.86630785139999844, -50.50000000000000000, -137.0552959530000123 ) ) ;
#18750 = DIRECTION ( 'NONE',  ( 0.000000000000000000, -4.253943788710456142E-15, -1.000000000000000000 ) ) ;
#18751 = ORIENTED_EDGE ( 'NONE', *, *, #21337, .T. ) ;
#18752 = EDGE_CURVE ( 'NONE', #20549, #12827, #21661, .T. ) ;
#18753 = DIRECTION ( 'NONE',  ( 1.000000000000000000, 0.000000000000000000, -4.430318231639999944E-12 ) ) ;
#18754 = ORIENTED_EDGE ( 'NONE', *, *, #3134, .T. ) ;
#18755 = LINE ( 'NONE', #9922, #17791 ) ;
#18756 = ORIENTED_EDGE ( 'NONE', *, *, #12733, .T. ) ;
#18757 = CARTESIAN_POINT ( 'NONE',  ( -27.77832206610000298, 37.03059619289999915, -147.6270870419999710 ) ) ;
#18758 = ORIENTED_EDGE ( 'NONE', *, *, #22749, .T. ) ;
#18759 = CARTESIAN_POINT ( 'NONE',  ( -21.73453520646456028, 32.91403690881655564, -144.3663112597476186 ) ) ;
#18760 = ORIENTED_EDGE ( 'NONE', *, *, #14743, .T. ) ;
#18761 = CARTESIAN_POINT ( 'NONE',  ( -17.92191803000494588, -43.78524365307784905, -150.0552959529999839 ) ) ;
#18762 = ORIENTED_EDGE ( 'NONE', *, *, #19643, .F. ) ;
#18763 = ORIENTED_EDGE ( 'NONE', *, *, #3128, .T. ) ;
#18764 = CARTESIAN_POINT ( 'NONE',  ( -27.66970514971757922, 40.84802520247237823, -146.1653953613356975 ) ) ;
#18765 = CARTESIAN_POINT ( 'NONE',  ( -46.50000000000000000, 37.00000000000000000, -149.0552959529999839 ) ) ;
#18766 = DIRECTION ( 'NONE',  ( 1.526468026909999897E-13, 8.159623473500000156E-13, 1.000000000000000000 ) ) ;
#18767 = LINE ( 'NONE', #12938, #4506 ) ;
#18768 = CARTESIAN_POINT ( 'NONE',  ( -6.323999170589999608, 34.61896835509999448, -147.3311432729999808 ) ) ;
#18769 = LINE ( 'NONE', #7582, #18196 ) ;
#18770 = ORIENTED_EDGE ( 'NONE', *, *, #20825, .F. ) ;
#18771 = FACE_OUTER_BOUND ( 'NONE', #11875, .T. ) ;
#18772 = CARTESIAN_POINT ( 'NONE',  ( 9.689837539793540344, 37.91893336569569328, -146.3818244917540312 ) ) ;
#18773 = CARTESIAN_POINT ( 'NONE',  ( -26.61707828802657261, 36.92896776167481221, -139.7487649555727671 ) ) ;
#18774 = ORIENTED_EDGE ( 'NONE', *, *, #19122, .T. ) ;
#18775 = CARTESIAN_POINT ( 'NONE',  ( -11.42599417689999974, 41.52668172479999953, -143.7505393120000292 ) ) ;
#18776 = EDGE_CURVE ( 'NONE', #7197, #18490, #7476, .T. ) ;
#18777 = CIRCLE ( 'NONE', #22967, 1.000000000000000888 ) ;
#18778 = DIRECTION ( 'NONE',  ( 0.000000000000000000, 1.000000000000000000, 0.000000000000000000 ) ) ;
#18779 = DIRECTION ( 'NONE',  ( 1.000000000000000000, 0.000000000000000000, -4.430318231639999944E-12 ) ) ;
#18780 = VERTEX_POINT ( 'NONE', #1565 ) ;
#18781 = PLANE ( 'NONE',  #17775 ) ;
#18782 = EDGE_CURVE ( 'NONE', #17090, #8499, #10500, .T. ) ;
#18783 = DIRECTION ( 'NONE',  ( -1.000000000000000000, 0.000000000000000000, 2.257453483404482811E-12 ) ) ;
#18784 = ORIENTED_EDGE ( 'NONE', *, *, #17386, .T. ) ;
#18785 = CARTESIAN_POINT ( 'NONE',  ( 2.531727043930000143, -11.80034048859999807, -148.0552959529999839 ) ) ;
#18786 = DIRECTION ( 'NONE',  ( 1.000000000000000000, 1.164156988989999824E-17, 2.507771768019999718E-12 ) ) ;
#18787 = VERTEX_POINT ( 'NONE', #1435 ) ;
#18788 = DIRECTION ( 'NONE',  ( -2.257144641399999941E-12, 0.000000000000000000, -1.000000000000000000 ) ) ;
#18789 = CARTESIAN_POINT ( 'NONE',  ( -21.18194668304453288, 41.60546844456856519, -144.5792247508281605 ) ) ;
#18790 = VERTEX_POINT ( 'NONE', #10559 ) ;
#18791 = CARTESIAN_POINT ( 'NONE',  ( -27.02696672876702522, 36.03294499660979966, -148.2622105679788547 ) ) ;
#18792 = CARTESIAN_POINT ( 'NONE',  ( 20.50000000000000000, 22.50000000000000000, -136.0552959530000123 ) ) ;
#18793 = ORIENTED_EDGE ( 'NONE', *, *, #17903, .F. ) ;
#18794 = CARTESIAN_POINT ( 'NONE',  ( 27.18320006080000084, 0.9999999999989999111, -148.5552959529999839 ) ) ;
#18795 = DIRECTION ( 'NONE',  ( -0.9800948705872890576, 0.1985297072190584933, -1.238441759210365047E-14 ) ) ;
#18796 = LINE ( 'NONE', #15106, #19369 ) ;
#18797 = VERTEX_POINT ( 'NONE', #19872 ) ;
#18798 = DIRECTION ( 'NONE',  ( -2.257144641399999941E-12, 0.000000000000000000, -1.000000000000000000 ) ) ;
#18799 = CARTESIAN_POINT ( 'NONE',  ( -15.92012808077673469, -44.20103055062003961, -136.0552959529640873 ) ) ;
#18800 = ORIENTED_EDGE ( 'NONE', *, *, #4547, .F. ) ;
#18801 = EDGE_CURVE ( 'NONE', #2700, #14669, #16060, .T. ) ;
#18802 = B_SPLINE_CURVE_WITH_KNOTS ( 'NONE', 3,
 ( #22335, #18651, #14723, #9588, #21990, #16861, #5681, #12937, #4253, #11489, #3910, #18418, #2126, #16621, #331, #7577, #14852, #22109 ),
 .UNSPECIFIED., .F., .F.,
 ( 4, 2, 2, 2, 2, 2, 2, 2, 4 ),
 ( 0.000000000000000000, 0.1249999999999998057, 0.2499999999999998335, 0.3749999999999998335, 0.4999999999999998890, 0.6249999999999998890, 0.7499999999999998890, 0.8750000000000000000, 1.000000000000000000 ),
 .UNSPECIFIED. ) ;
#18803 = VERTEX_POINT ( 'NONE', #14033 ) ;
#18804 = FACE_OUTER_BOUND ( 'NONE', #16007, .T. ) ;
#18805 = CARTESIAN_POINT ( 'NONE',  ( -30.53444983796061152, 41.17095381152200417, -144.9066004078397896 ) ) ;
#18806 = CARTESIAN_POINT ( 'NONE',  ( 23.50000000000000000, -20.50000000000000000, -136.0552959530000123 ) ) ;
#18807 = LINE ( 'NONE', #6544, #6446 ) ;
#18808 = ORIENTED_EDGE ( 'NONE', *, *, #15155, .T. ) ;
#18809 = SURFACE_SIDE_STYLE ('',( #16556 ) ) ;
#18810 = EDGE_CURVE ( 'NONE', #20903, #15726, #12241, .T. ) ;
#18811 = CARTESIAN_POINT ( 'NONE',  ( 17.58326321919999558, -18.99156222550000095, -146.5552959529999839 ) ) ;
#18812 = LINE ( 'NONE', #21081, #9025 ) ;
#18813 = DIRECTION ( 'NONE',  ( 0.000000000000000000, 0.000000000000000000, 1.000000000000000000 ) ) ;
#18814 = DIRECTION ( 'NONE',  ( 2.602084704489999637E-17, -1.000000000000000000, -4.426606872070000353E-37 ) ) ;
#18815 = VECTOR ( 'NONE', #16180, 1000.000000000000000 ) ;
#18816 = CARTESIAN_POINT ( 'NONE',  ( -34.35824191590000254, -34.50000000000000000, -141.0657682190000060 ) ) ;
#18817 = CARTESIAN_POINT ( 'NONE',  ( -17.68978131335611081, 36.92028947728231714, -140.0842674915936072 ) ) ;
#18818 = EDGE_CURVE ( 'NONE', #23189, #6609, #20771, .T. ) ;
#18819 = DIRECTION ( 'NONE',  ( 2.257171095940000041E-12, -7.494005416210000121E-16, 1.000000000000000000 ) ) ;
#18820 = LINE ( 'NONE', #2769, #23269 ) ;
#18821 = CARTESIAN_POINT ( 'NONE',  ( -34.50000000000000000, 76.00000000000000000, -144.0552959529999839 ) ) ;
#18822 = VERTEX_POINT ( 'NONE', #5691 ) ;
#18823 = CARTESIAN_POINT ( 'NONE',  ( -9.611837139799998653, 32.98927337829999829, -146.0840312179999785 ) ) ;
#18824 = LINE ( 'NONE', #11787, #11873 ) ;
#18825 = ORIENTED_EDGE ( 'NONE', *, *, #5568, .T. ) ;
#18826 = EDGE_CURVE ( 'NONE', #70, #4750, #912, .T. ) ;
#18827 = EDGE_CURVE ( 'NONE', #473, #2813, #9253, .T. ) ;
#18829 = AXIS2_PLACEMENT_3D ( 'NONE', #18576, #15362, #5842 ) ;
#18828 = CARTESIAN_POINT ( 'NONE',  ( -21.78746107307105362, 34.94849561060180321, -146.8035918688234176 ) ) ;
#18830 = AXIS2_PLACEMENT_3D ( 'NONE', #1852, #16578, #7310 ) ;
#18831 = LINE ( 'NONE', #883, #10986 ) ;
#18832 = ORIENTED_EDGE ( 'NONE', *, *, #1543, .F. ) ;
#18833 = CARTESIAN_POINT ( 'NONE',  ( -12.14655699389284038, 34.61986692078499317, -147.3395159944840032 ) ) ;
#18834 = ADVANCED_FACE ( 'NONE', ( #8136 ), #4465, .T. ) ;
#18835 = DIRECTION ( 'NONE',  ( -1.000000000000000000, 0.000000000000000000, -2.516505522483685870E-12 ) ) ;
#18836 = EDGE_CURVE ( 'NONE', #15103, #1341, #4821, .T. ) ;
#18837 = DIRECTION ( 'NONE',  ( 0.000000000000000000, 0.000000000000000000, 1.000000000000000000 ) ) ;
#18838 = LINE ( 'NONE', #17046, #20802 ) ;
#18839 = LINE ( 'NONE', #2547, #14657 ) ;
#18840 = CARTESIAN_POINT ( 'NONE',  ( -8.462973826026347623, 36.94736262684725858, -140.5165674475847766 ) ) ;
#18841 = VERTEX_POINT ( 'NONE', #1914 ) ;
#18842 = CARTESIAN_POINT ( 'NONE',  ( -27.47244207672152072, 35.09215423528084443, -148.2237751110284023 ) ) ;
#18843 = ORIENTED_EDGE ( 'NONE', *, *, #11108, .T. ) ;
#18844 = AXIS2_PLACEMENT_3D ( 'NONE', #239, #7135, #14278 ) ;
#18845 = DIRECTION ( 'NONE',  ( 0.000000000000000000, 0.000000000000000000, 1.000000000000000000 ) ) ;
#18846 = CARTESIAN_POINT ( 'NONE',  ( 8.750000000030000891, -2.273736754430000208E-12, -136.0552959530000123 ) ) ;
#18847 = VECTOR ( 'NONE', #3739, 1000.000000000000000 ) ;
#18848 = CARTESIAN_POINT ( 'NONE',  ( -6.366307851350000213, -50.50000000000000000, -137.0552959530000123 ) ) ;
#18849 = ADVANCED_FACE ( 'NONE', ( #11702 ), #9136, .F. ) ;
#18850 = ORIENTED_EDGE ( 'NONE', *, *, #6937, .T. ) ;
#18851 = DIRECTION ( 'NONE',  ( 0.000000000000000000, -1.000000000000000000, 0.000000000000000000 ) ) ;
#18852 = PLANE ( 'NONE',  #2310 ) ;
#18853 = ORIENTED_EDGE ( 'NONE', *, *, #8377, .F. ) ;
#18854 = CARTESIAN_POINT ( 'NONE',  ( 13.80479507505236825, 18.53689086730539515, -136.0552959530164969 ) ) ;
#18855 = EDGE_CURVE ( 'NONE', #2146, #8510, #16416, .T. ) ;
#18856 = CARTESIAN_POINT ( 'NONE',  ( -17.71126569018024099, 40.30718541996639459, -145.9389846959718113 ) ) ;
#18857 = EDGE_CURVE ( 'NONE', #21113, #11661, #18537, .T. ) ;
#18858 = DIRECTION ( 'NONE',  ( -1.000000000000000000, 0.000000000000000000, 0.000000000000000000 ) ) ;
#18859 = FACE_OUTER_BOUND ( 'NONE', #18131, .T. ) ;
#18860 = VECTOR ( 'NONE', #11293, 1000.000000000000000 ) ;
#18861 = CARTESIAN_POINT ( 'NONE',  ( -25.70078729276114515, 36.31727625687209837, -140.6851652563827031 ) ) ;
#18862 = ORIENTED_EDGE ( 'NONE', *, *, #9796, .T. ) ;
#18863 = CARTESIAN_POINT ( 'NONE',  ( 22.36721601470000209, -21.34320095609999868, -147.5552959529999839 ) ) ;
#18864 = ORIENTED_EDGE ( 'NONE', *, *, #20251, .T. ) ;
#18865 = FACE_OUTER_BOUND ( 'NONE', #17274, .T. ) ;
#18866 = ORIENTED_EDGE ( 'NONE', *, *, #23008, .T. ) ;
#18867 = CARTESIAN_POINT ( 'NONE',  ( -9.876524491812205042, -22.81279121395682807, -144.5552959529502743 ) ) ;
#18868 = ORIENTED_EDGE ( 'NONE', *, *, #23137, .T. ) ;
#18869 = DIRECTION ( 'NONE',  ( 2.257144641399999941E-12, -4.009147065140000298E-51, 1.000000000000000000 ) ) ;
#18870 = ORIENTED_EDGE ( 'NONE', *, *, #8082, .F. ) ;
#18871 = FACE_OUTER_BOUND ( 'NONE', #302, .T. ) ;
#18872 = ORIENTED_EDGE ( 'NONE', *, *, #8617, .T. ) ;
#18873 = ORIENTED_EDGE ( 'NONE', *, *, #2698, .F. ) ;
#18874 = CARTESIAN_POINT ( 'NONE',  ( -27.57732796661917973, 40.50144436171580509, -145.9796795535191336 ) ) ;
#18875 = DIRECTION ( 'NONE',  ( 1.000000000000000000, -5.094701932209999624E-24, -2.257144641399999941E-12 ) ) ;
#18876 = VECTOR ( 'NONE', #2032, 1000.000000000000227 ) ;
#18877 = CARTESIAN_POINT ( 'NONE',  ( -10.76224745929999926, 37.97907322949999553, -139.7231730900000173 ) ) ;
#18878 = CYLINDRICAL_SURFACE ( 'NONE', #6273, 8.000000000000000000 ) ;
#18879 = DIRECTION ( 'NONE',  ( 2.257144641399999941E-12, 0.000000000000000000, -1.000000000000000000 ) ) ;
#18880 = EDGE_CURVE ( 'NONE', #20938, #22607, #13065, .T. ) ;
#18881 = CARTESIAN_POINT ( 'NONE',  ( -7.728596210859999260, 38.74386132360000090, -140.2295773360000055 ) ) ;
#18882 = ORIENTED_EDGE ( 'NONE', *, *, #10349, .F. ) ;
#18883 = DIRECTION ( 'NONE',  ( 0.000000000000000000, 0.000000000000000000, -1.000000000000000000 ) ) ;
#18884 = EDGE_CURVE ( 'NONE', #13434, #11590, #12950, .T. ) ;
#18885 = DIRECTION ( 'NONE',  ( 0.000000000000000000, -1.000000000000000000, 8.159623473500000156E-13 ) ) ;
#18886 = CARTESIAN_POINT ( 'NONE',  ( -18.07392865290000117, -34.50000000000000000, -144.8157682190000060 ) ) ;
#18887 = ORIENTED_EDGE ( 'NONE', *, *, #4487, .F. ) ;
#18888 = VECTOR ( 'NONE', #9195, 1000.000000000000227 ) ;
#18889 = CARTESIAN_POINT ( 'NONE',  ( -18.60901166351236924, 37.01038625230344792, -148.6497975989735494 ) ) ;
#18890 = CARTESIAN_POINT ( 'NONE',  ( -3.500000000000000000, 44.50000000000000000, -151.0552959529999839 ) ) ;
#18891 = AXIS2_PLACEMENT_3D ( 'NONE', #7507, #9520, #9631 ) ;
#18892 = ORIENTED_EDGE ( 'NONE', *, *, #668, .F. ) ;
#18893 = CARTESIAN_POINT ( 'NONE',  ( 6.500000000000000000, 28.00000000000000000, -150.0552959529999839 ) ) ;
#18894 = ORIENTED_EDGE ( 'NONE', *, *, #14085, .T. ) ;
#18895 = CARTESIAN_POINT ( 'NONE',  ( -35.47299999999999898, 11.36725231429999816, -145.4935725690000083 ) ) ;
#18896 = PLANE ( 'NONE',  #462 ) ;
#18897 = ORIENTED_EDGE ( 'NONE', *, *, #3451, .T. ) ;
#18898 = CARTESIAN_POINT ( 'NONE',  ( -14.34860313725863712, 37.92192996123270632, -139.4939723716648530 ) ) ;
#18899 = APPLICATION_CONTEXT ( 'automotive_design' ) ;
#18900 = CARTESIAN_POINT ( 'NONE',  ( -19.92532084488878752, 37.01154022405491872, -139.3892291660223748 ) ) ;
#18901 = EDGE_LOOP ( 'NONE', ( #17064, #1831, #11632, #1993 ) ) ;
#18902 = PRESENTATION_STYLE_ASSIGNMENT (( #4631 ) ) ;
#18903 = CARTESIAN_POINT ( 'NONE',  ( -28.90798551749711720, 37.01360947634791643, -139.5686590453459814 ) ) ;
#18904 = CARTESIAN_POINT ( 'NONE',  ( 6.500000000000000000, 20.50000000000000000, -150.0552959529999839 ) ) ;
#18905 = VERTEX_POINT ( 'NONE', #18199 ) ;
#18906 = CARTESIAN_POINT ( 'NONE',  ( -25.86630785139999844, -51.50000000000000000, -136.0552959530000123 ) ) ;
#18907 = DIRECTION ( 'NONE',  ( -1.263593756457750072E-14, 0.000000000000000000, 1.000000000000000000 ) ) ;
#18908 = ORIENTED_EDGE ( 'NONE', *, *, #127, .F. ) ;
#18909 = CARTESIAN_POINT ( 'NONE',  ( -2.499999999839999987, 20.50000000000000000, -139.5552959529999839 ) ) ;
#18910 = VECTOR ( 'NONE', #21814, 1000.000000000000000 ) ;
#18911 = ORIENTED_EDGE ( 'NONE', *, *, #17375, .F. ) ;
#18912 = ADVANCED_FACE ( 'NONE', ( #7471 ), #5577, .T. ) ;
#18913 = DIRECTION ( 'NONE',  ( 0.000000000000000000, -1.000000000000000000, 0.000000000000000000 ) ) ;
#18914 = STYLED_ITEM ( 'NONE', ( #3218 ), #19750 ) ;
#18915 = CARTESIAN_POINT ( 'NONE',  ( -16.46194989540135367, -43.39058393986235984, -136.0552959529628083 ) ) ;
#18916 = EDGE_CURVE ( 'NONE', #154, #10363, #11262, .T. ) ;
#18917 = ORIENTED_EDGE ( 'NONE', *, *, #3473, .F. ) ;
#18918 = ORIENTED_EDGE ( 'NONE', *, *, #2486, .T. ) ;
#18919 = CARTESIAN_POINT ( 'NONE',  ( 1.499999999999999112, -3.107300918301282522, -150.0552959529999839 ) ) ;
#18921 = DIRECTION ( 'NONE',  ( 1.000000000000000000, 3.994014904670000134E-29, -2.423380700840000070E-27 ) ) ;
#18920 = B_SPLINE_CURVE_WITH_KNOTS ( 'NONE', 3,
 ( #20688, #17229, #4383, #15335, #2839, #10069, #17347, #22592, #6281, #13535, #8292, #15566, #3426, #23298, #6872, #18059, #17823, #1540 ),
 .UNSPECIFIED., .F., .F.,
 ( 4, 2, 2, 2, 2, 2, 2, 2, 4 ),
 ( 0.000000000000000000, 0.1250000000000000000, 0.2500000000000000000, 0.3750000000000000000, 0.5000000000000000000, 0.6250000000000000000, 0.7500000000000000000, 0.8750000000000000000, 1.000000000000000000 ),
 .UNSPECIFIED. ) ;
#18922 = CARTESIAN_POINT ( 'NONE',  ( -13.40552595227776855, 37.07358616897465708, -140.3498584192782062 ) ) ;
#18923 = DIRECTION ( 'NONE',  ( -2.257242012349999735E-12, 0.000000000000000000, 1.000000000000000000 ) ) ;
#18924 = ORIENTED_EDGE ( 'NONE', *, *, #5752, .T. ) ;
#18925 = CARTESIAN_POINT ( 'NONE',  ( 15.50000000000000000, 33.50000000000000000, -136.5552959530000123 ) ) ;
#18926 = LINE ( 'NONE', #13098, #4392 ) ;
#18927 = AXIS2_PLACEMENT_3D ( 'NONE', #22732, #20964, #4655 ) ;
#18928 = PLANE ( 'NONE',  #5996 ) ;
#18929 = CARTESIAN_POINT ( 'NONE',  ( -11.38486064709999823, 36.95668670079999885, -140.3965526140000009 ) ) ;
#18930 = CARTESIAN_POINT ( 'NONE',  ( -23.10566298545525754, 41.14502951780827544, -141.7794040582555510 ) ) ;
#18931 = VECTOR ( 'NONE', #3056, 1000.000000000000000 ) ;
#18932 = CARTESIAN_POINT ( 'NONE',  ( 19.13369214859999801, -51.50000000000000000, -143.0552959529999839 ) ) ;
#18933 = PLANE ( 'NONE',  #5661 ) ;
#18934 = DIRECTION ( 'NONE',  ( 1.000000000000000000, 0.000000000000000000, -2.257171095940000041E-12 ) ) ;
#18935 = LINE ( 'NONE', #3790, #19470 ) ;
#18936 = DIRECTION ( 'NONE',  ( 0.000000000000000000, 0.000000000000000000, -1.000000000000000000 ) ) ;
#18937 = ORIENTED_EDGE ( 'NONE', *, *, #4304, .F. ) ;
#18938 = FACE_OUTER_BOUND ( 'NONE', #6448, .T. ) ;
#18939 = CARTESIAN_POINT ( 'NONE',  ( -33.50000000000000000, 48.00000000000000000, -137.5552959530000123 ) ) ;
#18940 = CARTESIAN_POINT ( 'NONE',  ( 19.13369214859999801, -50.50000000000000000, -136.0552959530000123 ) ) ;
#18941 = EDGE_CURVE ( 'NONE', #13141, #5742, #125, .T. ) ;
#18942 = ORIENTED_EDGE ( 'NONE', *, *, #1669, .F. ) ;
#18943 = VECTOR ( 'NONE', #14962, 1000.000000000000000 ) ;
#18944 = AXIS2_PLACEMENT_3D ( 'NONE', #13928, #2993, #15365 ) ;
#18945 = DIRECTION ( 'NONE',  ( 0.000000000000000000, 0.000000000000000000, 1.000000000000000000 ) ) ;
#18946 = LINE ( 'NONE', #10006, #14807 ) ;
#18947 = ORIENTED_EDGE ( 'NONE', *, *, #9531, .T. ) ;
#18948 = CARTESIAN_POINT ( 'NONE',  ( -23.03778781520344054, 40.78628791112352303, -141.9896475654208245 ) ) ;
#18949 = CARTESIAN_POINT ( 'NONE',  ( -35.07300000000000040, 16.55147016440000129, -144.5552959529999839 ) ) ;
#18950 = AXIS2_PLACEMENT_3D ( 'NONE', #22965, #4642, #8187 ) ;
#18951 = EDGE_CURVE ( 'NONE', #16256, #3279, #18427, .T. ) ;
#18952 = DIRECTION ( 'NONE',  ( -1.000000000000000000, 0.000000000000000000, 2.257144641399999941E-12 ) ) ;
#18953 = LINE ( 'NONE', #9892, #21251 ) ;
#18954 = CARTESIAN_POINT ( 'NONE',  ( 23.63070326403130039, -30.71011948576827066, -147.5552959530019166 ) ) ;
#18955 = DIRECTION ( 'NONE',  ( 0.7633862853691523176, -0.6459422414661291079, 0.000000000000000000 ) ) ;
#18956 = CARTESIAN_POINT ( 'NONE',  ( -8.925445592990907784, 40.16747143530070474, -142.1449410552589825 ) ) ;
#18957 = ORIENTED_EDGE ( 'NONE', *, *, #21161, .T. ) ;
#18958 = FACE_OUTER_BOUND ( 'NONE', #22545, .T. ) ;
#18959 = VECTOR ( 'NONE', #23429, 1000.000000000000000 ) ;
#18960 = EDGE_CURVE ( 'NONE', #11473, #3916, #23068, .T. ) ;
#18961 = AXIS2_PLACEMENT_3D ( 'NONE', #5496, #4795, #17287 ) ;
#18962 = VERTEX_POINT ( 'NONE', #22003 ) ;
#18963 = CARTESIAN_POINT ( 'NONE',  ( -13.82353779650958003, 34.78290842727324161, -141.1681162278995885 ) ) ;
#18964 = LINE ( 'NONE', #898, #12612 ) ;
#18965 = DIRECTION ( 'NONE',  ( -0.1185248058649825964, -0.4964755458219273776, -0.8599208700778737668 ) ) ;
#18966 = VECTOR ( 'NONE', #366, 1000.000000000000000 ) ;
#18967 = EDGE_CURVE ( 'NONE', #16505, #23292, #23010, .T. ) ;
#18968 = ORIENTED_EDGE ( 'NONE', *, *, #15897, .F. ) ;
#18969 = CIRCLE ( 'NONE', #7559, 9.000000000000000000 ) ;
#18970 = DIRECTION ( 'NONE',  ( -2.257144641399999941E-12, 8.049635416090000264E-35, -1.000000000000000000 ) ) ;
#18971 = LINE ( 'NONE', #1143, #9486 ) ;
#18972 = ORIENTED_EDGE ( 'NONE', *, *, #4567, .T. ) ;
#18973 = CARTESIAN_POINT ( 'NONE',  ( 23.50000000000000000, -20.50000000000000000, -136.0552959530000123 ) ) ;
#18974 = CARTESIAN_POINT ( 'NONE',  ( -18.79127896110195906, 39.63013235846046456, -147.4718746916258851 ) ) ;
#18975 = CARTESIAN_POINT ( 'NONE',  ( 7.051758037318819561, 36.60562334003225970, -146.5244709269151429 ) ) ;
#18976 = VECTOR ( 'NONE', #23109, 1000.000000000000000 ) ;
#18977 = DIRECTION ( 'NONE',  ( 8.956391184260000029E-12, -9.094947017729999296E-13, 1.000000000000000000 ) ) ;
#18978 = EDGE_CURVE ( 'NONE', #11661, #11512, #6345, .T. ) ;
#18979 = AXIS2_PLACEMENT_3D ( 'NONE', #17259, #13687, #967 ) ;
#18980 = CARTESIAN_POINT ( 'NONE',  ( -25.07725372939999886, 36.26300138690000097, -147.8685835880000070 ) ) ;
#18981 = EDGE_CURVE ( 'NONE', #19891, #16708, #4823, .T. ) ;
#18982 = DIRECTION ( 'NONE',  ( 2.842170943040000002E-14, 3.570477247189999985E-13, 1.000000000000000000 ) ) ;
#18983 = EDGE_CURVE ( 'NONE', #1242, #4356, #10285, .T. ) ;
#18984 = VECTOR ( 'NONE', #6530, 999.9999999999998863 ) ;
#18985 = AXIS2_PLACEMENT_3D ( 'NONE', #6662, #5361, #10693 ) ;
#18986 = ORIENTED_EDGE ( 'NONE', *, *, #9948, .T. ) ;
#18987 = FACE_OUTER_BOUND ( 'NONE', #15308, .T. ) ;
#18988 = ORIENTED_EDGE ( 'NONE', *, *, #18165, .F. ) ;
#18989 = DIRECTION ( 'NONE',  ( -2.839308199620000013E-14, -3.568879590630000244E-13, -1.000000000000000000 ) ) ;
#18990 = ADVANCED_FACE ( 'NONE', ( #13863 ), #15766, .T. ) ;
#18991 = VERTEX_POINT ( 'NONE', #8386 ) ;
#18992 = DIRECTION ( 'NONE',  ( 1.000000000000000000, 0.000000000000000000, -2.256131789327549967E-12 ) ) ;
#18993 = EDGE_CURVE ( 'NONE', #2014, #14816, #23263, .T. ) ;
#18994 = ORIENTED_EDGE ( 'NONE', *, *, #1940, .F. ) ;
#18995 = DIRECTION ( 'NONE',  ( 1.000000000000000000, 2.602084747549999882E-17, 0.000000000000000000 ) ) ;
#18996 = ORIENTED_EDGE ( 'NONE', *, *, #23539, .T. ) ;
#18997 = EDGE_CURVE ( 'NONE', #13875, #10751, #3270, .T. ) ;
#18998 = ORIENTED_EDGE ( 'NONE', *, *, #20825, .T. ) ;
#18999 = CYLINDRICAL_SURFACE ( 'NONE', #5683, 2.999999999999999112 ) ;
#19000 = EDGE_CURVE ( 'NONE', #20206, #5119, #15838, .T. ) ;
#19001 = DIRECTION ( 'NONE',  ( 0.7071067811865499042, 0.7071067811865451302, 1.776356839400251071E-12 ) ) ;
#19002 = DIRECTION ( 'NONE',  ( 0.000000000000000000, 1.000000000000000000, 0.000000000000000000 ) ) ;
#19003 = CIRCLE ( 'NONE', #4565, 7.000000000000000000 ) ;
#19004 = AXIS2_PLACEMENT_3D ( 'NONE', #20299, #6119, #547 ) ;
#19005 = DIRECTION ( 'NONE',  ( 0.000000000000000000, 1.000000000000000000, -2.245315044999999693E-12 ) ) ;
#19006 = CARTESIAN_POINT ( 'NONE',  ( 4.128836048080000154, -25.17057797350000214, -147.5552959529999839 ) ) ;
#19007 = ORIENTED_EDGE ( 'NONE', *, *, #3029, .T. ) ;
#19008 = FACE_OUTER_BOUND ( 'NONE', #18551, .T. ) ;
#19009 = CARTESIAN_POINT ( 'NONE',  ( 9.168738215927051627, 38.34300703367464536, -146.1639638664460961 ) ) ;
#19010 = CARTESIAN_POINT ( 'NONE',  ( 25.42371301058693689, 37.28076054106433901, -150.0552959529999839 ) ) ;
#19011 = ORIENTED_EDGE ( 'NONE', *, *, #2138, .F. ) ;
#19012 = DIRECTION ( 'NONE',  ( 8.954614827420000395E-12, -9.112710586119999183E-13, 1.000000000000000000 ) ) ;
#19013 = CARTESIAN_POINT ( 'NONE',  ( -23.31991597950000283, 35.31558869410000057, -140.3324749399999973 ) ) ;
#19014 = ORIENTED_EDGE ( 'NONE', *, *, #5889, .T. ) ;
#19015 = DIRECTION ( 'NONE',  ( -1.000000000000000000, 0.000000000000000000, 0.000000000000000000 ) ) ;
#19016 = VECTOR ( 'NONE', #22709, 1000.000000000000000 ) ;
#19017 = AXIS2_PLACEMENT_3D ( 'NONE', #21124, #8374, #10147 ) ;
#19018 = VERTEX_POINT ( 'NONE', #6715 ) ;
#19019 = LINE ( 'NONE', #17346, #7222 ) ;
#19020 = CARTESIAN_POINT ( 'NONE',  ( -46.29070078880000239, 45.00000000000000000, -147.5552959540000018 ) ) ;
#19021 = VERTEX_POINT ( 'NONE', #4585 ) ;
#19022 = CARTESIAN_POINT ( 'NONE',  ( -14.31404048463135936, 38.45176613018843881, -140.7319883511322018 ) ) ;
#19023 = ADVANCED_FACE ( 'NONE', ( #23028 ), #11825, .T. ) ;
#19024 = CARTESIAN_POINT ( 'NONE',  ( -25.44349950013895878, 35.21826511855759634, -139.9516901550857995 ) ) ;
#19025 = ORIENTED_EDGE ( 'NONE', *, *, #22575, .F. ) ;
#19026 = CARTESIAN_POINT ( 'NONE',  ( 27.02097087391203800, -17.55867353012727250, -143.5552959530038208 ) ) ;
#19027 = EDGE_LOOP ( 'NONE', ( #4500, #9340, #6775, #17196, #3376, #280, #19352, #16632 ) ) ;
#19028 = DIRECTION ( 'NONE',  ( 1.000000000000000000, 0.000000000000000000, 2.516505522483685870E-12 ) ) ;
#19029 = LINE ( 'NONE', #10205, #865 ) ;
#19030 = VERTEX_POINT ( 'NONE', #10395 ) ;
#19031 = CARTESIAN_POINT ( 'NONE',  ( -7.500000000000000000, 19.50000000000000000, -150.0552959529999839 ) ) ;
#19032 = EDGE_LOOP ( 'NONE', ( #15347, #10045, #23363 ) ) ;
#19033 = CARTESIAN_POINT ( 'NONE',  ( 6.000000000140000012, 32.99305018889999275, -146.5552959529999839 ) ) ;
#19034 = DIRECTION ( 'NONE',  ( -0.9919007982877544594, 0.1270149847699686418, 0.000000000000000000 ) ) ;
#19035 = VERTEX_POINT ( 'NONE', #10035 ) ;
#19036 = AXIS2_PLACEMENT_3D ( 'NONE', #12799, #20310, #16271 ) ;
#19037 = VECTOR ( 'NONE', #21583, 1000.000000000000000 ) ;
#19038 = VERTEX_POINT ( 'NONE', #17311 ) ;
#19039 = FACE_OUTER_BOUND ( 'NONE', #5404, .T. ) ;
#19040 = CARTESIAN_POINT ( 'NONE',  ( -9.812199629310001114, -24.40642616239999896, -146.5552959529999839 ) ) ;
#19041 = PLANE ( 'NONE',  #20058 ) ;
#19042 = LINE ( 'NONE', #13920, #2654 ) ;
#19043 = ORIENTED_EDGE ( 'NONE', *, *, #8899, .T. ) ;
#19044 = CARTESIAN_POINT ( 'NONE',  ( -15.92022845431896982, -41.79886907580737443, -136.0552959529640589 ) ) ;
#19045 = EDGE_CURVE ( 'NONE', #5687, #5601, #1026, .T. ) ;
#19046 = LINE ( 'NONE', #13335, #22622 ) ;
#19047 = DIRECTION ( 'NONE',  ( 0.000000000000000000, -2.252420471819999940E-12, 1.000000000000000000 ) ) ;
#19048 = LINE ( 'NONE', #15601, #18686 ) ;
#19049 = EDGE_CURVE ( 'NONE', #14758, #4470, #22792, .T. ) ;
#19050 = LINE ( 'NONE', #13694, #14001 ) ;
#19051 = ADVANCED_FACE ( 'NONE', ( #15876 ), #23146, .T. ) ;
#19052 = VECTOR ( 'NONE', #12166, 1000.000000000000227 ) ;
#19053 = ORIENTED_EDGE ( 'NONE', *, *, #16635, .T. ) ;
#19054 = VECTOR ( 'NONE', #23446, 1000.000000000000000 ) ;
#19055 = DIRECTION ( 'NONE',  ( 0.000000000000000000, 0.000000000000000000, 1.000000000000000000 ) ) ;
#19056 = CARTESIAN_POINT ( 'NONE',  ( -16.65899329396956219, 33.56230705803076830, -145.9446936787583411 ) ) ;
#19057 = CARTESIAN_POINT ( 'NONE',  ( -4.954580150880754097, 37.98786518323144179, -139.3930060029525748 ) ) ;
#19058 = CARTESIAN_POINT ( 'NONE',  ( -10.00000000000000000, 48.50000000000000000, -151.0552959529999839 ) ) ;
#19059 = CARTESIAN_POINT ( 'NONE',  ( 27.68320006080000084, -34.50000000000000000, -148.5552959529999839 ) ) ;
#19060 = ORIENTED_EDGE ( 'NONE', *, *, #4687, .F. ) ;
#19061 = CARTESIAN_POINT ( 'NONE',  ( -9.137845891433649115, 36.16121174422281825, -147.5839243320841945 ) ) ;
#19062 = DIRECTION ( 'NONE',  ( 1.000000000000000000, 0.000000000000000000, -2.257453483404485639E-12 ) ) ;
#19063 = CARTESIAN_POINT ( 'NONE',  ( -25.86630785139999844, -50.50000000000000000, -137.0552959530000123 ) ) ;
#19064 = VERTEX_POINT ( 'NONE', #4704 ) ;
#19065 = ADVANCED_FACE ( 'NONE', ( #6835 ), #14102, .T. ) ;
#19066 = CARTESIAN_POINT ( 'NONE',  ( 19.13369214859999801, 51.50000000000000000, -149.5552959529999839 ) ) ;
#19067 = CARTESIAN_POINT ( 'NONE',  ( -13.86630785140000022, 50.50000000000000000, -142.8052959529999839 ) ) ;
#19068 = COLOUR_RGB ( '', 0.08235294, 0.09019608, 0.10196078) ;
#19069 = VECTOR ( 'NONE', #22051, 1000.000000000000000 ) ;
#19070 = DIRECTION ( 'NONE',  ( 0.000000000000000000, 0.000000000000000000, 1.000000000000000000 ) ) ;
#19071 = ORIENTED_EDGE ( 'NONE', *, *, #16949, .T. ) ;
#19072 = AXIS2_PLACEMENT_3D ( 'NONE', #19800, #18361, #16341 ) ;
#19073 = CARTESIAN_POINT ( 'NONE',  ( -13.40552595227776855, 37.07358616897465708, -140.3498584192782062 ) ) ;
#19074 = DIRECTION ( 'NONE',  ( -2.507771768020000122E-12, -0.000000000000000000, 1.000000000000000000 ) ) ;
#19075 = DIRECTION ( 'NONE',  ( 0.000000000000000000, 0.000000000000000000, 1.000000000000000000 ) ) ;
#19076 = DIRECTION ( 'NONE',  ( 0.000000000000000000, -1.000000000000000000, 0.000000000000000000 ) ) ;
#19077 = CARTESIAN_POINT ( 'NONE',  ( -5.537589236589999686, 40.52957482200000072, -146.1175057039999956 ) ) ;
#19078 = DIRECTION ( 'NONE',  ( 0.000000000000000000, 1.000000000000000000, 0.000000000000000000 ) ) ;
#19079 = B_SPLINE_CURVE_WITH_KNOTS ( 'NONE', 3,
 ( #18122, #14200, #17889, #21933, #12392, #20150, #15983, #7049, #1606, #3844, #12639, #8940, #8825, #16104, #7167, #10839, #19798, #16219 ),
 .UNSPECIFIED., .F., .F.,
 ( 4, 2, 2, 2, 2, 2, 2, 2, 4 ),
 ( 0.000000000000000000, 0.1250000000000000000, 0.2500000000000000000, 0.3750000000000000000, 0.5000000000000000000, 0.6250000000000000000, 0.7500000000000000000, 0.8750000000000000000, 1.000000000000000000 ),
 .UNSPECIFIED. ) ;
#19080 = CARTESIAN_POINT ( 'NONE',  ( 9.444192711117707972, -34.64608312524905642, -150.0552959529999555 ) ) ;
#19081 = EDGE_CURVE ( 'NONE', #21363, #20751, #5062, .T. ) ;
#19082 = VERTEX_POINT ( 'NONE', #12892 ) ;
#19083 = ADVANCED_FACE ( 'NONE', ( #19928 ), #5414, .F. ) ;
#19084 =( BOUNDED_CURVE ( )  B_SPLINE_CURVE ( 5, ( #17555, #1271, #8494, #15764, #6712, #4939 ),
 .UNSPECIFIED., .F., .F. ) 
 B_SPLINE_CURVE_WITH_KNOTS ( ( 6, 6 ),
 ( 0.000000000000000000, 1.570796326505558671 ),
 .UNSPECIFIED. ) 
 CURVE ( )  GEOMETRIC_REPRESENTATION_ITEM ( )  RATIONAL_B_SPLINE_CURVE ( ( 1.000000000000000000, 0.6000000000737055750, 0.4000000000737055639, 0.3000000000552791590, 0.2500000000368527431, 0.2500000000000000000 ) ) 
 REPRESENTATION_ITEM ( '' )  );
#19085 = ORIENTED_EDGE ( 'NONE', *, *, #437, .F. ) ;
#19086 = CARTESIAN_POINT ( 'NONE',  ( -6.713398844220000328, 32.91877557720000169, -144.5413327229999823 ) ) ;
#19087 = CARTESIAN_POINT ( 'NONE',  ( -25.84964047060000070, 38.84307078620000198, -139.9757795270000145 ) ) ;
#19088 = PLANE ( 'NONE',  #13844 ) ;
#19089 = VECTOR ( 'NONE', #8515, 1000.000000000000000 ) ;
#19090 = EDGE_LOOP ( 'NONE', ( #11358, #6518, #21789, #181 ) ) ;
#19091 = PLANE ( 'NONE',  #23187 ) ;
#19092 = CARTESIAN_POINT ( 'NONE',  ( -14.80611810279999929, 41.62812440830000327, -144.5263372940000011 ) ) ;
#19093 = ORIENTED_EDGE ( 'NONE', *, *, #2257, .F. ) ;
#19094 = DIRECTION ( 'NONE',  ( 0.000000000000000000, -1.000000000000000000, 2.257144641399999941E-12 ) ) ;
#19095 = CARTESIAN_POINT ( 'NONE',  ( -17.86540859994439145, 40.46207760455489222, -144.3551126902200110 ) ) ;
#19096 = CARTESIAN_POINT ( 'NONE',  ( 8.500000000060001781, 35.50000000000000000, -146.0552959529999839 ) ) ;
#19097 = ADVANCED_FACE ( 'NONE', ( #21726 ), #14220, .T. ) ;
#19098 = DIRECTION ( 'NONE',  ( 1.000000000000000000, -2.312964634635743450E-15, 0.000000000000000000 ) ) ;
#19099 = CARTESIAN_POINT ( 'NONE',  ( -25.38678224704462494, 37.07582353397745578, -140.0279244688365168 ) ) ;
#19100 = CARTESIAN_POINT ( 'NONE',  ( 6.000000000000000000, -3.500000000000000000, -150.0552959529999839 ) ) ;
#19101 = AXIS2_PLACEMENT_3D ( 'NONE', #15675, #926, #19002 ) ;
#19102 = ORIENTED_EDGE ( 'NONE', *, *, #524, .T. ) ;
#19103 = CARTESIAN_POINT ( 'NONE',  ( -2.500000000000000000, 37.00000000000000000, -151.0552959529999839 ) ) ;
#19104 = EDGE_CURVE ( 'NONE', #7140, #5042, #4056, .T. ) ;
#19105 = ORIENTED_EDGE ( 'NONE', *, *, #6442, .T. ) ;
#19106 = CARTESIAN_POINT ( 'NONE',  ( -26.86963863710373701, 36.92213009831746007, -147.8538433455846359 ) ) ;
#19107 = VERTEX_POINT ( 'NONE', #12413 ) ;
#19108 = FACE_OUTER_BOUND ( 'NONE', #18547, .T. ) ;
#19109 = EDGE_LOOP ( 'NONE', ( #6354, #20458, #13790, #15891 ) ) ;
#19110 = FACE_OUTER_BOUND ( 'NONE', #4978, .T. ) ;
#19111 = EDGE_LOOP ( 'NONE', ( #18305, #8886, #12759, #13784 ) ) ;
#19112 = ORIENTED_EDGE ( 'NONE', *, *, #18652, .T. ) ;
#19113 = DIRECTION ( 'NONE',  ( 2.257146850379999957E-12, 0.000000000000000000, 1.000000000000000000 ) ) ;
#19114 = ADVANCED_FACE ( 'NONE', ( #3384 ), #12660, .F. ) ;
#19115 = FACE_OUTER_BOUND ( 'NONE', #21593, .T. ) ;
#19116 = CARTESIAN_POINT ( 'NONE',  ( -4.499999999949999996, 40.00000000000000000, -150.0552959529999839 ) ) ;
#19117 = DIRECTION ( 'NONE',  ( -0.1146332952500066227, -0.9934078757590583120, -9.947598300640582187E-14 ) ) ;
#19118 = DIRECTION ( 'NONE',  ( 0.000000000000000000, 1.000000000000000000, 0.000000000000000000 ) ) ;
#19119 = LINE ( 'NONE', #19006, #1512 ) ;
#19120 = ORIENTED_EDGE ( 'NONE', *, *, #1231, .F. ) ;
#19121 = CARTESIAN_POINT ( 'NONE',  ( -27.36723106709999698, 36.02973761859999513, -148.4771530680000353 ) ) ;
#19122 = EDGE_CURVE ( 'NONE', #13199, #22055, #8961, .T. ) ;
#19123 = FACE_OUTER_BOUND ( 'NONE', #12286, .T. ) ;
#19124 = ADVANCED_FACE ( 'NONE', ( #23380 ), #7075, .F. ) ;
#19125 = DIRECTION ( 'NONE',  ( 5.094701932209999624E-24, 1.000000000000000000, 0.000000000000000000 ) ) ;
#19126 = EDGE_LOOP ( 'NONE', ( #726, #19014, #18613, #15866 ) ) ;
#19127 = EDGE_CURVE ( 'NONE', #9406, #18690, #19688, .T. ) ;
#19128 = EDGE_CURVE ( 'NONE', #16693, #6748, #12028, .T. ) ;
#19129 = LINE ( 'NONE', #14223, #18509 ) ;
#19130 = DIRECTION ( 'NONE',  ( 1.000000000000000000, 0.000000000000000000, -2.257453483404482811E-12 ) ) ;
#19131 = EDGE_LOOP ( 'NONE', ( #23452, #16872, #12649, #921 ) ) ;
#19132 = CARTESIAN_POINT ( 'NONE',  ( 1.133692148650000009, -51.50000000000000000, -136.5552959530000123 ) ) ;
#19133 = AXIS2_PLACEMENT_3D ( 'NONE', #1664, #23071, #14374 ) ;
#19134 = PLANE ( 'NONE',  #21510 ) ;
#19135 = ORIENTED_EDGE ( 'NONE', *, *, #8959, .T. ) ;
#19136 = FACE_OUTER_BOUND ( 'NONE', #17635, .T. ) ;
#19137 = LINE ( 'NONE', #10193, #17935 ) ;
#19138 = ORIENTED_EDGE ( 'NONE', *, *, #9734, .F. ) ;
#19139 = VECTOR ( 'NONE', #9561, 1000.000000000000000 ) ;
#19140 = FACE_OUTER_BOUND ( 'NONE', #14761, .T. ) ;
#19141 = CARTESIAN_POINT ( 'NONE',  ( -24.99941573887451796, 32.27097850041364069, -144.5668997986605007 ) ) ;
#19142 = ORIENTED_EDGE ( 'NONE', *, *, #20869, .F. ) ;
#19143 = PLANE ( 'NONE',  #161 ) ;
#19144 = EDGE_LOOP ( 'NONE', ( #12739, #10042, #3516, #13803, #2809 ) ) ;
#19145 = DIRECTION ( 'NONE',  ( 0.000000000000000000, 0.000000000000000000, 1.000000000000000000 ) ) ;
#19146 = DIRECTION ( 'NONE',  ( -0.9968185442904002880, 0.07970438983373201447, 8.712538262633493651E-14 ) ) ;
#19147 = VERTEX_POINT ( 'NONE', #16580 ) ;
#19148 = CARTESIAN_POINT ( 'NONE',  ( -32.50000000000000000, 26.00000000000000000, -141.5552959529999839 ) ) ;
#19149 = VERTEX_POINT ( 'NONE', #1976 ) ;
#19150 = DIRECTION ( 'NONE',  ( 2.510584333019999972E-12, 0.000000000000000000, -1.000000000000000000 ) ) ;
#19151 = DIRECTION ( 'NONE',  ( 1.000000000000000000, 0.000000000000000000, 0.000000000000000000 ) ) ;
#19152 = ORIENTED_EDGE ( 'NONE', *, *, #4898, .F. ) ;
#19153 = CIRCLE ( 'NONE', #15744, 6.000000000000001776 ) ;
#19154 = ADVANCED_FACE ( 'NONE', ( #20047 ), #66, .F. ) ;
#19155 = EDGE_LOOP ( 'NONE', ( #20780, #23015, #5916, #23070, #215 ) ) ;
#19156 = DIRECTION ( 'NONE',  ( 2.257146850379999957E-12, 0.000000000000000000, 1.000000000000000000 ) ) ;
#19157 = DIRECTION ( 'NONE',  ( 7.389987738588579788E-14, 0.000000000000000000, 1.000000000000000000 ) ) ;
#19158 = CYLINDRICAL_SURFACE ( 'NONE', #6742, 1.500000000000001332 ) ;
#19159 = CARTESIAN_POINT ( 'NONE',  ( -9.334216945200001447, -17.19633444960000190, -146.5552959529999839 ) ) ;
#19160 = EDGE_LOOP ( 'NONE', ( #21342, #1280, #2382, #1632 ) ) ;
#19161 = CARTESIAN_POINT ( 'NONE',  ( -15.39058393985465223, -41.53805010459524283, -136.0552959529652242 ) ) ;
#19162 = FACE_OUTER_BOUND ( 'NONE', #16192, .T. ) ;
#19163 = CARTESIAN_POINT ( 'NONE',  ( -9.873006318519999880, -23.84776512999999909, -142.5552959529999839 ) ) ;
#19164 = CARTESIAN_POINT ( 'NONE',  ( 17.21087225569999646, -22.66053313549999970, -145.0552959529999839 ) ) ;
#19165 = CARTESIAN_POINT ( 'NONE',  ( -17.08912089869999917, -18.00000000000000000, -147.1421200419999877 ) ) ;
#19166 = CARTESIAN_POINT ( 'NONE',  ( 4.500000000009999113, -2.000000000000000000, -136.5552959530000123 ) ) ;
#19167 = ORIENTED_EDGE ( 'NONE', *, *, #21530, .F. ) ;
#19168 = CARTESIAN_POINT ( 'NONE',  ( -17.13033207850000039, 36.08498863180000171, -139.6042211940000186 ) ) ;
#19169 = VECTOR ( 'NONE', #3344, 1000.000000000000000 ) ;
#19170 = DIRECTION ( 'NONE',  ( -0.9954742291034677226, 0.09503188512734457583, 4.502513436702118395E-12 ) ) ;
#19171 = DIRECTION ( 'NONE',  ( 1.000000000000000000, 0.000000000000000000, -4.510281037539696830E-12 ) ) ;
#19172 = CARTESIAN_POINT ( 'NONE',  ( 23.50000000000000000, -20.50000000000000000, -142.5552959529999839 ) ) ;
#19173 = CARTESIAN_POINT ( 'NONE',  ( 23.00000000000000000, 19.50000000000000000, -137.0552959530000123 ) ) ;
#19174 = ORIENTED_EDGE ( 'NONE', *, *, #2755, .T. ) ;
#19175 = CARTESIAN_POINT ( 'NONE',  ( -9.447016884546547644, 33.25211036581616497, -145.9271147563237321 ) ) ;
#19176 = CARTESIAN_POINT ( 'NONE',  ( -4.499999999959999109, 34.00000000000000000, -153.0552959529999839 ) ) ;
#19177 = DIRECTION ( 'NONE',  ( -1.000000000000000000, 0.000000000000000000, 0.000000000000000000 ) ) ;
#19178 = ORIENTED_EDGE ( 'NONE', *, *, #1122, .T. ) ;
#19179 = PRESENTATION_STYLE_ASSIGNMENT (( #6328 ) ) ;
#19180 = EDGE_CURVE ( 'NONE', #947, #76, #5524, .T. ) ;
#19181 = CARTESIAN_POINT ( 'NONE',  ( -29.29455083639855673, 36.96746664034980512, -139.4767999530844520 ) ) ;
#19182 = LINE ( 'NONE', #2893, #4541 ) ;
#19183 = EDGE_LOOP ( 'NONE', ( #4384, #17442, #6583, #11524 ) ) ;
#19184 = CARTESIAN_POINT ( 'NONE',  ( -23.77821355560346817, 39.18276288788521811, -141.0264728964231153 ) ) ;
#19185 = DIRECTION ( 'NONE',  ( -1.000000000000000000, 0.000000000000000000, 2.254788948169999945E-12 ) ) ;
#19186 = DIRECTION ( 'NONE',  ( 1.000000000000000000, 0.000000000000000000, 0.000000000000000000 ) ) ;
#19187 = CARTESIAN_POINT ( 'NONE',  ( 16.16922456049999823, -22.27514461170000004, -147.5552959529999839 ) ) ;
#19188 = VECTOR ( 'NONE', #18145, 1000.000000000000000 ) ;
#19189 = CARTESIAN_POINT ( 'NONE',  ( -10.75221293931074129, 33.20739279160920177, -143.4848104350353992 ) ) ;
#19190 = CARTESIAN_POINT ( 'NONE',  ( 1.924079216156750372, 26.46241645103150475, -150.0552959529999839 ) ) ;
#19191 = CARTESIAN_POINT ( 'NONE',  ( -8.748495699880534104, 39.09191467989751345, -141.0690580214405259 ) ) ;
#19192 = VERTEX_POINT ( 'NONE', #20172 ) ;
#19193 =( NAMED_UNIT ( * ) SI_UNIT ( $, .STERADIAN. ) SOLID_ANGLE_UNIT ( ) );
#19194 = ORIENTED_EDGE ( 'NONE', *, *, #307, .F. ) ;
#19195 = CARTESIAN_POINT ( 'NONE',  ( -7.187032243693241895, 34.73215247832149544, -140.9426763503612676 ) ) ;
#19196 = DIRECTION ( 'NONE',  ( 1.000000000000000000, 0.000000000000000000, 0.000000000000000000 ) ) ;
#19197 = CARTESIAN_POINT ( 'NONE',  ( -20.76253627919999900, 39.57534689110000414, -140.5049880910000013 ) ) ;
#19198 = VERTEX_POINT ( 'NONE', #14456 ) ;
#19199 = CARTESIAN_POINT ( 'NONE',  ( -34.50000000000000000, 14.00000000000000000, -144.0552959529999839 ) ) ;
#19200 = CARTESIAN_POINT ( 'NONE',  ( -14.23530246729999860, 39.72954597060000026, -140.2988105550000171 ) ) ;
#19201 = CIRCLE ( 'NONE', #3636, 5.000000000000000000 ) ;
#19202 = ORIENTED_EDGE ( 'NONE', *, *, #2222, .F. ) ;
#19203 = CYLINDRICAL_SURFACE ( 'NONE', #16362, 0.7500000000000013323 ) ;
#19204 = EDGE_CURVE ( 'NONE', #634, #477, #10625, .T. ) ;
#19205 = CARTESIAN_POINT ( 'NONE',  ( -18.02589426845994680, 40.09893371072652002, -145.7828789349928229 ) ) ;
#19206 = LINE ( 'NONE', #22785, #5936 ) ;
#19207 = EDGE_CURVE ( 'NONE', #6404, #8234, #9072, .T. ) ;
#19208 = FACE_BOUND ( 'NONE', #18734, .T. ) ;
#19209 = LINE ( 'NONE', #2920, #5536 ) ;
#19210 = APPLICATION_CONTEXT ( 'automotive_design' ) ;
#19211 = CARTESIAN_POINT ( 'NONE',  ( -25.17085604102206275, 34.85061541308337496, -141.0238190163674687 ) ) ;
#19212 = DIRECTION ( 'NONE',  ( 1.000000000000000000, 0.000000000000000000, -2.259525899719999991E-12 ) ) ;
#19213 = PRODUCT_DEFINITION_SHAPE ( 'NONE', 'NONE',  #23541 ) ;
#19214 = CARTESIAN_POINT ( 'NONE',  ( -11.36739930689422451, 37.96852355311366978, -139.4217770014837754 ) ) ;
#19215 = EDGE_LOOP ( 'NONE', ( #3952, #21328, #12673, #2378 ) ) ;
#19216 = DIRECTION ( 'NONE',  ( 1.000000000000000000, 0.000000000000000000, -2.257171095940000041E-12 ) ) ;
#19217 = CIRCLE ( 'NONE', #618, 2.999999999999999112 ) ;
#19218 = EDGE_LOOP ( 'NONE', ( #6104, #1059, #19518, #3249 ) ) ;
#19219 = DIRECTION ( 'NONE',  ( 1.000000000000000000, 0.000000000000000000, -2.854859206178974232E-14 ) ) ;
#19220 = EDGE_LOOP ( 'NONE', ( #13437, #8523, #22518, #13566 ) ) ;
#19221 = DIRECTION ( 'NONE',  ( 1.000000000000000000, 0.000000000000000000, 0.000000000000000000 ) ) ;
#19222 = ORIENTED_EDGE ( 'NONE', *, *, #12301, .T. ) ;
#19223 = CARTESIAN_POINT ( 'NONE',  ( -0.9999999999639996862, 20.99262443222791319, -136.0552959529977954 ) ) ;
#19224 = VERTEX_POINT ( 'NONE', #8845 ) ;
#19225 = ORIENTED_EDGE ( 'NONE', *, *, #12168, .T. ) ;
#19226 = DIRECTION ( 'NONE',  ( 0.000000000000000000, -1.000000000000000000, 0.000000000000000000 ) ) ;
#19227 = CARTESIAN_POINT ( 'NONE',  ( -19.04867772230000256, 35.29145880730000329, -148.2212826610000036 ) ) ;
#19228 = CARTESIAN_POINT ( 'NONE',  ( -10.89103387395912215, 38.50335587980050889, -140.8674315661253331 ) ) ;
#19229 = DIRECTION ( 'NONE',  ( 2.257171095940000041E-12, 1.003664318210000046E-28, 1.000000000000000000 ) ) ;
#19230 = CARTESIAN_POINT ( 'NONE',  ( -6.808372428180324398, 32.54462665076120231, -143.6393730288246218 ) ) ;
#19231 = CARTESIAN_POINT ( 'NONE',  ( -9.353760014424715052, 38.97728680361760922, -148.4651161360701508 ) ) ;
#19232 = ORIENTED_EDGE ( 'NONE', *, *, #19, .T. ) ;
#19233 = DIRECTION ( 'NONE',  ( 0.000000000000000000, 2.257144641399999941E-12, -1.000000000000000000 ) ) ;
#19234 = CIRCLE ( 'NONE', #12777, 2.500000000000000444 ) ;
#19235 = EDGE_CURVE ( 'NONE', #2055, #12686, #3863, .T. ) ;
#19236 = VECTOR ( 'NONE', #3166, 1000.000000000000114 ) ;
#19237 = CARTESIAN_POINT ( 'NONE',  ( -31.75000000000000000, 1.000000000000000000, -150.0552959529999839 ) ) ;
#19238 = CARTESIAN_POINT ( 'NONE',  ( 24.33939095839631861, 38.90181682659950724, -150.0552959529999839 ) ) ;
#19239 = EDGE_LOOP ( 'NONE', ( #8141, #17949, #7935, #3893 ) ) ;
#19240 = ADVANCED_FACE ( 'NONE', ( #12535 ), #19816, .T. ) ;
#19241 = FACE_OUTER_BOUND ( 'NONE', #6703, .T. ) ;
#19242 = CARTESIAN_POINT ( 'NONE',  ( -14.47770030809999930, -34.50000000000000000, -148.5552959529999839 ) ) ;
#19243 = ORIENTED_EDGE ( 'NONE', *, *, #22294, .F. ) ;
#19244 = CARTESIAN_POINT ( 'NONE',  ( 6.500000000140000012, 20.50000000000000000, -147.5552959529999839 ) ) ;
#19245 = ORIENTED_EDGE ( 'NONE', *, *, #16286, .T. ) ;
#19246 = DIRECTION ( 'NONE',  ( 1.000000000000000000, 0.000000000000000000, 0.000000000000000000 ) ) ;
#19247 = CARTESIAN_POINT ( 'NONE',  ( 15.50000000000000000, 33.50000000000000000, -136.0552959530000123 ) ) ;
#19248 = ORIENTED_EDGE ( 'NONE', *, *, #5864, .F. ) ;
#19249 = FACE_OUTER_BOUND ( 'NONE', #20336, .T. ) ;
#19250 = VECTOR ( 'NONE', #14682, 1000.000000000000227 ) ;
#19251 = CARTESIAN_POINT ( 'NONE',  ( -26.11589873370086323, 33.33025833338455612, -142.0389129396357362 ) ) ;
#19252 = EDGE_LOOP ( 'NONE', ( #14137, #23075, #21386, #18094 ) ) ;
#19253 = FILL_AREA_STYLE_COLOUR ( '', #2405 ) ;
#19254 = EDGE_CURVE ( 'NONE', #18797, #2028, #3743, .T. ) ;
#19255 = CARTESIAN_POINT ( 'NONE',  ( -2.500000000000000000, 37.00000000000000000, -150.0552959529999839 ) ) ;
#19256 = VERTEX_POINT ( 'NONE', #18954 ) ;
#19257 = CARTESIAN_POINT ( 'NONE',  ( -11.68420994730000118, 39.25205177019999780, -141.0178453350000041 ) ) ;
#19258 = ADVANCED_FACE ( 'NONE', ( #14805 ), #13239, .F. ) ;
#19259 = DIRECTION ( 'NONE',  ( -0.7071067811865481278, -0.7071067811865469066, -1.776356839400246426E-12 ) ) ;
#19260 = ORIENTED_EDGE ( 'NONE', *, *, #12218, .T. ) ;
#19261 = CARTESIAN_POINT ( 'NONE',  ( -32.50000000000000000, 50.50000000000000000, -137.0552959530000123 ) ) ;
#19262 = EDGE_CURVE ( 'NONE', #9232, #7276, #10900, .T. ) ;
#19263 = ORIENTED_EDGE ( 'NONE', *, *, #14913, .T. ) ;
#19264 = CARTESIAN_POINT ( 'NONE',  ( 24.68320006080000084, -16.50000000000000000, -150.0552959529999839 ) ) ;
#19265 = EDGE_CURVE ( 'NONE', #19696, #4078, #3976, .T. ) ;
#19266 = CARTESIAN_POINT ( 'NONE',  ( -9.766576661180000229, -34.50000000000000000, -145.5657682190000060 ) ) ;
#19267 = ORIENTED_EDGE ( 'NONE', *, *, #21861, .F. ) ;
#19268 = AXIS2_PLACEMENT_3D ( 'NONE', #11675, #17286, #21103 ) ;
#19269 = COLOUR_RGB ( '', 0.09019608, 0.27058824, 0.51372549) ;
#19270 = ORIENTED_EDGE ( 'NONE', *, *, #13448, .F. ) ;
#19271 = CARTESIAN_POINT ( 'NONE',  ( 6.343640159924743394, -1.100999472805458401, -150.0552959529999839 ) ) ;
#19272 = CARTESIAN_POINT ( 'NONE',  ( -4.499999999919999105, 40.00000000000000000, -136.5552959530000123 ) ) ;
#19273 = EDGE_CURVE ( 'NONE', #760, #7372, #7530, .T. ) ;
#19274 = CARTESIAN_POINT ( 'NONE',  ( -13.69950222120749928, 37.97208955950073772, -139.6409136025020246 ) ) ;
#19275 = CARTESIAN_POINT ( 'NONE',  ( -32.50000000000000000, 47.00000000000000000, -141.5552959529999839 ) ) ;
#19276 = EDGE_LOOP ( 'NONE', ( #1663, #7078, #5869, #16144, #17129, #23036, #9201 ) ) ;
#19277 = DIRECTION ( 'NONE',  ( -1.000000000000000000, 0.000000000000000000, 0.000000000000000000 ) ) ;
#19278 = DIRECTION ( 'NONE',  ( 0.000000000000000000, -1.000000000000000000, 0.000000000000000000 ) ) ;
#19279 = EDGE_CURVE ( 'NONE', #4474, #9000, #5248, .T. ) ;
#19280 = DIRECTION ( 'NONE',  ( 0.000000000000000000, 0.000000000000000000, 1.000000000000000000 ) ) ;
#19281 = CARTESIAN_POINT ( 'NONE',  ( -14.80142434073996860, -41.50006722989636643, -150.0552959529999839 ) ) ;
#19282 = CARTESIAN_POINT ( 'NONE',  ( -21.35824191589999899, -32.00000000000000000, -146.2257682199999920 ) ) ;
#19283 = CARTESIAN_POINT ( 'NONE',  ( 12.50000000009097079, 24.10555127549999810, -147.5552959530157864 ) ) ;
#19284 = ORIENTED_EDGE ( 'NONE', *, *, #19721, .T. ) ;
#19285 = CARTESIAN_POINT ( 'NONE',  ( -16.72821278489138663, 35.17558473326719337, -139.6880632856704381 ) ) ;
#19286 = VECTOR ( 'NONE', #19307, 1000.000000000000000 ) ;
#19287 = EDGE_CURVE ( 'NONE', #14651, #7053, #7765, .T. ) ;
#19288 = FACE_OUTER_BOUND ( 'NONE', #604, .T. ) ;
#19289 = EDGE_CURVE ( 'NONE', #15072, #7782, #7112, .T. ) ;
#19290 = AXIS2_PLACEMENT_3D ( 'NONE', #10099, #969, #3106 ) ;
#19291 = DIRECTION ( 'NONE',  ( 1.000000000000000000, 0.000000000000000000, -1.527536832333223921E-13 ) ) ;
#19292 = CARTESIAN_POINT ( 'NONE',  ( 13.13369214859999978, -50.50000000000000000, -136.0552959530000123 ) ) ;
#19293 = LINE ( 'NONE', #19173, #10029 ) ;
#19294 = EDGE_CURVE ( 'NONE', #12291, #14669, #20746, .T. ) ;
#19295 = ORIENTED_EDGE ( 'NONE', *, *, #12083, .F. ) ;
#19296 = FACE_OUTER_BOUND ( 'NONE', #8942, .T. ) ;
#19297 = CARTESIAN_POINT ( 'NONE',  ( -7.499999999959999997, 19.50000000000000000, -136.0552959530000123 ) ) ;
#19298 = DIRECTION ( 'NONE',  ( -1.000000000000000000, 0.000000000000000000, 1.701177084980000217E-20 ) ) ;
#19299 = VERTEX_POINT ( 'NONE', #11450 ) ;
#19300 = CARTESIAN_POINT ( 'NONE',  ( 8.500000000060001781, 35.50000000000000000, -144.0552959529999839 ) ) ;
#19301 = LINE ( 'NONE', #14068, #8326 ) ;
#19302 = DIRECTION ( 'NONE',  ( 1.000000000000000000, 0.000000000000000000, 0.000000000000000000 ) ) ;
#19303 = EDGE_LOOP ( 'NONE', ( #15859, #8021, #7942, #4988 ) ) ;
#19304 = CARTESIAN_POINT ( 'NONE',  ( -23.25111789197735845, 40.11822973618910027, -142.3379301973523923 ) ) ;
#19305 = DIRECTION ( 'NONE',  ( 2.257144641399999941E-12, 0.000000000000000000, 1.000000000000000000 ) ) ;
#19306 = AXIS2_PLACEMENT_3D ( 'NONE', #22798, #11588, #6493 ) ;
#19307 = DIRECTION ( 'NONE',  ( 0.000000000000000000, 0.000000000000000000, -1.000000000000000000 ) ) ;
#19308 = CARTESIAN_POINT ( 'NONE',  ( 8.250850001128238631, 38.47921821292768385, -142.0398975025202333 ) ) ;
#19309 = ORIENTED_EDGE ( 'NONE', *, *, #10243, .F. ) ;
#19310 = CARTESIAN_POINT ( 'NONE',  ( -9.394775000179999225, 34.25903911019999981, -147.4808749560000081 ) ) ;
#19311 = DIRECTION ( 'NONE',  ( 0.9834926989016489207, 0.1809478134909354718, -4.411697319228424767E-12 ) ) ;
#19312 = CARTESIAN_POINT ( 'NONE',  ( -45.83792946319999828, 45.00000000000000000, -146.9594324700000243 ) ) ;
#19313 = CARTESIAN_POINT ( 'NONE',  ( 20.31210873290000052, -31.32069079449999904, -147.5552959529999839 ) ) ;
#19314 = VERTEX_POINT ( 'NONE', #13012 ) ;
#19315 = FACE_OUTER_BOUND ( 'NONE', #22672, .T. ) ;
#19316 = ADVANCED_FACE ( 'NONE', ( #13363 ), #22292, .T. ) ;
#19317 = EDGE_CURVE ( 'NONE', #16851, #954, #11066, .T. ) ;
#19318 = ORIENTED_EDGE ( 'NONE', *, *, #8608, .T. ) ;
#19319 = CARTESIAN_POINT ( 'NONE',  ( -6.817148331763788427, 33.23134552036847111, -143.6958372513363145 ) ) ;
#19320 = DIRECTION ( 'NONE',  ( -2.507771768020000122E-12, -0.000000000000000000, 1.000000000000000000 ) ) ;
#19321 = CARTESIAN_POINT ( 'NONE',  ( 11.68320006079999906, -20.50000000000000000, -148.5552959529999839 ) ) ;
#19322 = AXIS2_PLACEMENT_3D ( 'NONE', #14825, #9884, #12908 ) ;
#19323 = EDGE_LOOP ( 'NONE', ( #6621, #17223, #16133, #18303 ) ) ;
#19324 = LINE ( 'NONE', #4932, #11761 ) ;
#19325 = CARTESIAN_POINT ( 'NONE',  ( 3.000000000010000001, -3.500000000000000000, -136.0552959530000123 ) ) ;
#19326 = VECTOR ( 'NONE', #12018, 1000.000000000000000 ) ;
#19327 = ORIENTED_EDGE ( 'NONE', *, *, #23052, .F. ) ;
#19328 = CARTESIAN_POINT ( 'NONE',  ( -21.12162747662785733, 36.95220905036273962, -147.5578847871555581 ) ) ;
#19329 = AXIS2_PLACEMENT_3D ( 'NONE', #2027, #14154, #7004 ) ;
#19330 = CARTESIAN_POINT ( 'NONE',  ( -18.18725233745032455, 40.59074569709380853, -143.5523115782840193 ) ) ;
#19331 = CARTESIAN_POINT ( 'NONE',  ( -16.51085694111269930, -40.37864083493722234, -150.0552959529999555 ) ) ;
#19332 = EDGE_CURVE ( 'NONE', #9556, #8221, #7996, .T. ) ;
#19333 = CARTESIAN_POINT ( 'NONE',  ( -13.11071995283477420, 37.07027326795080313, -147.8134892432881884 ) ) ;
#19334 = DIRECTION ( 'NONE',  ( 0.000000000000000000, 1.000000000000000000, 0.000000000000000000 ) ) ;
#19335 = CARTESIAN_POINT ( 'NONE',  ( -24.20723148424393756, 36.23170097884169394, -147.4988838138595213 ) ) ;
#19336 = CARTESIAN_POINT ( 'NONE',  ( -13.86630785140000022, 51.00000000000000000, -137.0552959530000123 ) ) ;
#19337 = CARTESIAN_POINT ( 'NONE',  ( -1.752427223251484367, 43.49276203925820283, -136.0552959530039345 ) ) ;
#19338 = VECTOR ( 'NONE', #12469, 1000.000000000000000 ) ;
#19339 = CIRCLE ( 'NONE', #10204, 7.000000000000000888 ) ;
#19340 = ORIENTED_EDGE ( 'NONE', *, *, #21868, .F. ) ;
#19341 = CARTESIAN_POINT ( 'NONE',  ( -0.9999999999649999971, 20.50000000000000000, -136.5552959530000123 ) ) ;
#19342 = EDGE_CURVE ( 'NONE', #23304, #13585, #15279, .T. ) ;
#19343 = AXIS2_PLACEMENT_3D ( 'NONE', #3697, #17983, #16434 ) ;
#19344 = EDGE_LOOP ( 'NONE', ( #17993, #17894 ) ) ;
#19345 = ORIENTED_EDGE ( 'NONE', *, *, #20704, .F. ) ;
#19346 = ADVANCED_FACE ( 'NONE', ( #2199 ), #22413, .T. ) ;
#19347 = AXIS2_PLACEMENT_3D ( 'NONE', #7469, #14732, #3679 ) ;
#19348 = ORIENTED_EDGE ( 'NONE', *, *, #2565, .T. ) ;
#19349 = DIRECTION ( 'NONE',  ( -1.000000000000000000, 0.000000000000000000, 2.257120985840000117E-12 ) ) ;
#19350 = CARTESIAN_POINT ( 'NONE',  ( -28.94327676059999988, 35.53474617860000251, -140.7339624629999832 ) ) ;
#19351 = ADVANCED_FACE ( 'NONE', ( #533 ), #5866, .F. ) ;
#19352 = ORIENTED_EDGE ( 'NONE', *, *, #21701, .T. ) ;
#19353 = ORIENTED_EDGE ( 'NONE', *, *, #6208, .T. ) ;
#19354 = CARTESIAN_POINT ( 'NONE',  ( 8.995627988029999855, -17.23072307649999857, -145.5552959529999839 ) ) ;
#19355 = CARTESIAN_POINT ( 'NONE',  ( -19.19584323397005221, 36.24030718097106529, -148.2165564152711568 ) ) ;
#19356 = FACE_OUTER_BOUND ( 'NONE', #13622, .T. ) ;
#19357 = PRESENTATION_STYLE_ASSIGNMENT (( #3067 ) ) ;
#19358 = CARTESIAN_POINT ( 'NONE',  ( 31.50000000000000000, -36.53620104879999531, -137.0552959530000123 ) ) ;
#19359 = AXIS2_PLACEMENT_3D ( 'NONE', #22822, #22945, #23055 ) ;
#19360 = CARTESIAN_POINT ( 'NONE',  ( -8.343166633029998280, 41.26425690090000131, -144.5268661329999986 ) ) ;
#19361 = ORIENTED_EDGE ( 'NONE', *, *, #16022, .T. ) ;
#19362 = AXIS2_PLACEMENT_3D ( 'NONE', #4762, #13812, #1216 ) ;
#19363 = DIRECTION ( 'NONE',  ( 1.526468026911395108E-13, 8.159623473499890094E-13, 1.000000000000000000 ) ) ;
#19364 = VECTOR ( 'NONE', #13165, 1000.000000000000227 ) ;
#19365 =( BOUNDED_CURVE ( )  B_SPLINE_CURVE ( 5, ( #7242, #19969, #21650, #9126, #14149, #5212 ),
 .UNSPECIFIED., .F., .F. ) 
 B_SPLINE_CURVE_WITH_KNOTS ( ( 6, 6 ),
 ( 0.000000000000000000, 1.570796326852883729 ),
 .UNSPECIFIED. ) 
 CURVE ( )  GEOMETRIC_REPRESENTATION_ITEM ( )  RATIONAL_B_SPLINE_CURVE ( ( 1.000000000000000000, 0.5999999999852601018, 0.3999999999852600907, 0.2999999999889450542, 0.2499999999926300620, 0.2500000000000000000 ) ) 
 REPRESENTATION_ITEM ( '' )  );
#19366 = AXIS2_PLACEMENT_3D ( 'NONE', #21740, #5540, #21620 ) ;
#19367 = CARTESIAN_POINT ( 'NONE',  ( 5.255428470566348764, -4.810679582531388832, -136.0552959530016892 ) ) ;
#19368 = VECTOR ( 'NONE', #14138, 1000.000000000000000 ) ;
#19369 = VECTOR ( 'NONE', #4396, 1000.000000000000000 ) ;
#19370 = DIRECTION ( 'NONE',  ( 0.000000000000000000, 1.000000000000000000, 0.000000000000000000 ) ) ;
#19371 = ORIENTED_EDGE ( 'NONE', *, *, #2068, .F. ) ;
#19372 = CARTESIAN_POINT ( 'NONE',  ( -34.50000000000000000, 76.00000000000000000, -132.5552959530000123 ) ) ;
#19373 = ORIENTED_EDGE ( 'NONE', *, *, #7906, .F. ) ;
#19374 = FACE_OUTER_BOUND ( 'NONE', #12453, .T. ) ;
#19375 = FACE_OUTER_BOUND ( 'NONE', #17785, .T. ) ;
#19376 = VERTEX_POINT ( 'NONE', #20634 ) ;
#19377 = CARTESIAN_POINT ( 'NONE',  ( -23.54789306460687826, 36.93722613941783806, -139.7713821671024448 ) ) ;
#19378 = CARTESIAN_POINT ( 'NONE',  ( 6.500000000130000011, 24.50000000000000000, -150.5552959529999839 ) ) ;
#19379 = ORIENTED_EDGE ( 'NONE', *, *, #952, .T. ) ;
#19380 = ADVANCED_FACE ( 'NONE', ( #4440 ), #7652, .F. ) ;
#19381 = CARTESIAN_POINT ( 'NONE',  ( -14.80611810279999929, 41.62812440830000327, -144.5263372940000011 ) ) ;
#19382 = CARTESIAN_POINT ( 'NONE',  ( -25.91744746520000220, 33.58572460659999592, -142.1592104600000255 ) ) ;
#19383 = EDGE_CURVE ( 'NONE', #14999, #7495, #18838, .T. ) ;
#19384 = EDGE_LOOP ( 'NONE', ( #11991, #11856, #17979, #4358 ) ) ;
#19385 = VECTOR ( 'NONE', #2100, 1000.000000000000000 ) ;
#19386 = VECTOR ( 'NONE', #11137, 1000.000000000000000 ) ;
#19387 = EDGE_LOOP ( 'NONE', ( #17017, #4444 ) ) ;
#19388 = VECTOR ( 'NONE', #18088, 1000.000000000000000 ) ;
#19389 = CYLINDRICAL_SURFACE ( 'NONE', #9468, 2.999999999999999112 ) ;
#19390 = CIRCLE ( 'NONE', #776, 8.176568160360000448 ) ;
#19391 = FACE_OUTER_BOUND ( 'NONE', #10023, .T. ) ;
#19392 = ORIENTED_EDGE ( 'NONE', *, *, #17087, .T. ) ;
#19393 = DIRECTION ( 'NONE',  ( -0.9954742291034677226, 0.09503188512734457583, 4.502513436702118395E-12 ) ) ;
#19394 = PRODUCT_DEFINITION ( 'UNKNOWN', '', #21420, #8966 ) ;
#19395 = DIRECTION ( 'NONE',  ( -2.257146850379999957E-12, 0.000000000000000000, -1.000000000000000000 ) ) ;
#19396 = EDGE_CURVE ( 'NONE', #5071, #10763, #22697, .T. ) ;
#19397 = CARTESIAN_POINT ( 'NONE',  ( 20.50000000000000000, 19.50000000000000000, -136.0552959530000123 ) ) ;
#19398 = ORIENTED_EDGE ( 'NONE', *, *, #20348, .F. ) ;
#19399 = VECTOR ( 'NONE', #13773, 1000.000000000000000 ) ;
#19400 = LINE ( 'NONE', #9738, #7461 ) ;
#19401 = ADVANCED_FACE ( 'NONE', ( #20866, #17526 ), #17171, .F. ) ;
#19402 = DIRECTION ( 'NONE',  ( 0.000000000000000000, 0.000000000000000000, 1.000000000000000000 ) ) ;
#19403 = CARTESIAN_POINT ( 'NONE',  ( -14.35172583810447478, 40.49725901027402841, -146.1414193758190549 ) ) ;
#19404 = CARTESIAN_POINT ( 'NONE',  ( -6.599319970649999867, -19.98386714700000155, -145.5552959529999839 ) ) ;
#19405 = ORIENTED_EDGE ( 'NONE', *, *, #5961, .F. ) ;
#19406 = DIRECTION ( 'NONE',  ( 0.000000000000000000, 0.000000000000000000, 1.000000000000000000 ) ) ;
#19407 = DIRECTION ( 'NONE',  ( 0.000000000000000000, -1.000000000000000000, 0.000000000000000000 ) ) ;
#19408 = LINE ( 'NONE', #8906, #3828 ) ;
#19409 = DIRECTION ( 'NONE',  ( -1.211690350420779919E-27, -2.765629237169220318E-27, 1.000000000000000000 ) ) ;
#19410 = CARTESIAN_POINT ( 'NONE',  ( -2.203055323360000095, -15.74846988260000025, -142.5552959529999839 ) ) ;
#19411 = DIRECTION ( 'NONE',  ( -2.257144641399999941E-12, 8.049635416090000264E-35, -1.000000000000000000 ) ) ;
#19412 = EDGE_CURVE ( 'NONE', #16477, #22408, #21332, .T. ) ;
#19413 = ORIENTED_EDGE ( 'NONE', *, *, #2109, .F. ) ;
#19414 = CARTESIAN_POINT ( 'NONE',  ( -32.50000000000000000, 20.50000000000000000, -151.0552959529999839 ) ) ;
#19415 = CARTESIAN_POINT ( 'NONE',  ( 10.50000000010000001, 24.50000000000000000, -150.5552959529999839 ) ) ;
#19416 = DIRECTION ( 'NONE',  ( -2.839308199620000013E-14, -3.568879590630000244E-13, -1.000000000000000000 ) ) ;
#19417 = CARTESIAN_POINT ( 'NONE',  ( -8.008464111600000379, 33.29536412539999901, -142.0809313899999893 ) ) ;
#19418 = CARTESIAN_POINT ( 'NONE',  ( 32.00000000000000000, 20.96379895120000114, -137.0552959530000123 ) ) ;
#19419 = VERTEX_POINT ( 'NONE', #8113 ) ;
#19420 = DIRECTION ( 'NONE',  ( -1.000000000000000000, 0.000000000000000000, 0.000000000000000000 ) ) ;
#19421 = ADVANCED_FACE ( 'NONE', ( #12277 ), #9326, .F. ) ;
#19422 = CARTESIAN_POINT ( 'NONE',  ( 14.00000000000000000, 20.50000000000000000, -136.0552959530000123 ) ) ;
#19423 = ORIENTED_EDGE ( 'NONE', *, *, #9952, .F. ) ;
#19424 = CARTESIAN_POINT ( 'NONE',  ( -28.70612892851496056, 35.15950212976387235, -139.8035036602401817 ) ) ;
#19425 = FACE_OUTER_BOUND ( 'NONE', #5529, .T. ) ;
#19426 = ORIENTED_EDGE ( 'NONE', *, *, #15963, .T. ) ;
#19427 = CARTESIAN_POINT ( 'NONE',  ( -23.71856152630000025, 38.62313066519999438, -140.3058339320000130 ) ) ;
#19428 = EDGE_CURVE ( 'NONE', #8477, #11000, #6731, .T. ) ;
#19429 = FACE_OUTER_BOUND ( 'NONE', #8587, .T. ) ;
#19430 = ADVANCED_FACE ( 'NONE', ( #19905 ), #21564, .F. ) ;
#19431 = MANIFOLD_SOLID_BREP ( 'lock_assembly.1\\Product1.1\\spring.1\\PartBody', #61 ) ;
#19432 = CARTESIAN_POINT ( 'NONE',  ( -31.00000000000000000, 19.50000000000000000, -149.5552959529999839 ) ) ;
#19433 = DIRECTION ( 'NONE',  ( 0.000000000000000000, -4.148443855749999753E-27, -1.000000000000000000 ) ) ;
#19434 = ORIENTED_EDGE ( 'NONE', *, *, #8625, .F. ) ;
#19435 = CARTESIAN_POINT ( 'NONE',  ( -9.611837139799998653, 32.98927337829999829, -146.0840312179999785 ) ) ;
#19436 = CIRCLE ( 'NONE', #22084, 2.000000000000000000 ) ;
#19437 = VECTOR ( 'NONE', #12785, 1000.000000000000000 ) ;
#19438 = CARTESIAN_POINT ( 'NONE',  ( 16.74346552629999962, -18.31657829129999726, -147.5552959529999839 ) ) ;
#19439 = AXIS2_PLACEMENT_3D ( 'NONE', #4661, #11900, #2997 ) ;
#19440 = EDGE_CURVE ( 'NONE', #13274, #4135, #16333, .T. ) ;
#19441 = LINE ( 'NONE', #6811, #7142 ) ;
#19442 = DIRECTION ( 'NONE',  ( 0.1985297072190585210, 0.9800948705872890576, -8.292396948122451413E-13 ) ) ;
#19443 = EDGE_CURVE ( 'NONE', #6729, #1522, #21457, .T. ) ;
#19444 = ORIENTED_EDGE ( 'NONE', *, *, #956, .T. ) ;
#19445 = FILL_AREA_STYLE ('',( #17533 ) ) ;
#19446 = SURFACE_STYLE_FILL_AREA ( #21112 ) ;
#19447 = VERTEX_POINT ( 'NONE', #3837 ) ;
#19448 = CARTESIAN_POINT ( 'NONE',  ( -7.406300769258751693, 33.57817176939022374, -144.5322665435940053 ) ) ;
#19449 = CARTESIAN_POINT ( 'NONE',  ( -26.95224972460000146, 39.68365438100000375, -147.7577323689999957 ) ) ;
#19450 = CARTESIAN_POINT ( 'NONE',  ( 10.94499944859915530, -21.50000000000000355, -148.5552959529999839 ) ) ;
#19451 = ORIENTED_EDGE ( 'NONE', *, *, #529, .T. ) ;
#19452 = FACE_OUTER_BOUND ( 'NONE', #15511, .T. ) ;
#19453 = CARTESIAN_POINT ( 'NONE',  ( -15.90886514219999981, -1.500000000000000000, -148.5657682190000060 ) ) ;
#19454 = VECTOR ( 'NONE', #19442, 1000.000000000000114 ) ;
#19455 = VECTOR ( 'NONE', #7516, 1000.000000000000000 ) ;
#19456 = ORIENTED_EDGE ( 'NONE', *, *, #14108, .F. ) ;
#19457 = AXIS2_PLACEMENT_3D ( 'NONE', #14990, #9378, #13430 ) ;
#19458 = CARTESIAN_POINT ( 'NONE',  ( -21.40343141177097053, 37.68083471479108226, -147.3689155900011372 ) ) ;
#19459 = CARTESIAN_POINT ( 'NONE',  ( 19.00000000000000000, 33.50000000000000000, -150.0552959529999839 ) ) ;
#19460 = DIRECTION ( 'NONE',  ( 4.511946372079999833E-12, -1.314504061159999897E-13, 1.000000000000000000 ) ) ;
#19461 = CARTESIAN_POINT ( 'NONE',  ( 7.976419552989963080, -46.35121046038157289, -136.0552959530180033 ) ) ;
#19462 = LINE ( 'NONE', #410, #23391 ) ;
#19463 = EDGE_CURVE ( 'NONE', #1863, #22853, #22042, .T. ) ;
#19464 = CARTESIAN_POINT ( 'NONE',  ( -17.55745234320252024, 36.93608508457233341, -140.4812394865590761 ) ) ;
#19465 = DIRECTION ( 'NONE',  ( 2.257144641399999941E-12, -8.049635416090000264E-35, 1.000000000000000000 ) ) ;
#19466 = LINE ( 'NONE', #10747, #22283 ) ;
#19467 = VERTEX_POINT ( 'NONE', #9284 ) ;
#19468 = PLANE ( 'NONE',  #14401 ) ;
#19469 = AXIS2_PLACEMENT_3D ( 'NONE', #9717, #18786, #13658 ) ;
#19470 = VECTOR ( 'NONE', #17628, 1000.000000000000000 ) ;
#19471 = UNCERTAINTY_MEASURE_WITH_UNIT (LENGTH_MEASURE( 1.000000000000000082E-05 ), #12419, 'distance_accuracy_value', 'NONE');
#19472 = AXIS2_PLACEMENT_3D ( 'NONE', #20944, #19146, #13670 ) ;
#19473 = EDGE_LOOP ( 'NONE', ( #19940, #4622, #18295, #23155 ) ) ;
#19474 =( NAMED_UNIT ( * ) PLANE_ANGLE_UNIT ( ) SI_UNIT ( $, .RADIAN. ) );
#19475 = MANIFOLD_SOLID_BREP ( 'lock_assembly.1\\Product1.1\\Part2.1\\PartBody', #15254 ) ;
#19476 = ORIENTED_EDGE ( 'NONE', *, *, #12699, .F. ) ;
#19477 = FACE_OUTER_BOUND ( 'NONE', #2498, .T. ) ;
#19478 = LINE ( 'NONE', #1515, #17547 ) ;
#19479 = ORIENTED_EDGE ( 'NONE', *, *, #10482, .T. ) ;
#19480 = VERTEX_POINT ( 'NONE', #13446 ) ;
#19481 = DIRECTION ( 'NONE',  ( 1.000000000000000000, 0.000000000000000000, 0.000000000000000000 ) ) ;
#19482 = CARTESIAN_POINT ( 'NONE',  ( -13.86630785140000022, -51.50000000000000000, -137.0552959530000123 ) ) ;
#19483 = CARTESIAN_POINT ( 'NONE',  ( -3.500000000000000000, 42.50000000000000000, -150.0552959529999839 ) ) ;
#19484 = DIRECTION ( 'NONE',  ( 0.002160933882609249439, 0.9999976651796518290, 8.911241827866908793E-13 ) ) ;
#19485 = CARTESIAN_POINT ( 'NONE',  ( -6.713398844220000328, 32.91877557720000169, -144.5413327229999823 ) ) ;
#19486 = ORIENTED_EDGE ( 'NONE', *, *, #1289, .T. ) ;
#19487 = LINE ( 'NONE', #13644, #18570 ) ;
#19488 =( GEOMETRIC_REPRESENTATION_CONTEXT ( 3 ) GLOBAL_UNCERTAINTY_ASSIGNED_CONTEXT ( ( #3057 ) ) GLOBAL_UNIT_ASSIGNED_CONTEXT ( ( #7536, #3871, #21732 ) ) REPRESENTATION_CONTEXT ( 'NONE', 'WORKASPACE' ) );
#19489 = AXIS2_PLACEMENT_3D ( 'NONE', #8218, #21445, #3125 ) ;
#19490 = EDGE_CURVE ( 'NONE', #17829, #23163, #15089, .T. ) ;
#19491 = CARTESIAN_POINT ( 'NONE',  ( -16.50000000000000000, -43.00000000000000000, -145.5552959529999839 ) ) ;
#19492 = DIRECTION ( 'NONE',  ( -2.507771768019999718E-12, -1.592654864209999947E-17, 1.000000000000000000 ) ) ;
#19493 = VERTEX_POINT ( 'NONE', #2063 ) ;
#19494 = DIRECTION ( 'NONE',  ( 1.000000000000000000, 0.000000000000000000, -2.257453483404485639E-12 ) ) ;
#19495 = ORIENTED_EDGE ( 'NONE', *, *, #11116, .T. ) ;
#19496 = CARTESIAN_POINT ( 'NONE',  ( -20.93854596069999729, 37.74500530009999721, -147.9603137869999898 ) ) ;
#19497 = CARTESIAN_POINT ( 'NONE',  ( 31.82297112080000190, 40.41789419139999495, -136.0552959530000123 ) ) ;
#19498 = ORIENTED_EDGE ( 'NONE', *, *, #14572, .T. ) ;
#19499 = CARTESIAN_POINT ( 'NONE',  ( -23.32853373983441969, 36.96341023004794835, -139.4571126577996836 ) ) ;
#19500 = DIRECTION ( 'NONE',  ( 0.000000000000000000, 1.000000000000000000, 0.000000000000000000 ) ) ;
#19501 = ORIENTED_EDGE ( 'NONE', *, *, #6960, .T. ) ;
#19502 = CARTESIAN_POINT ( 'NONE',  ( -15.46613156833100078, 36.99333119719623397, -147.5584717933785726 ) ) ;
#19503 = CARTESIAN_POINT ( 'NONE',  ( -25.46021907539999773, 33.59345108530000346, -146.1038275270000213 ) ) ;
#19504 = PRESENTATION_LAYER_ASSIGNMENT (  '', '', ( #20638 ) ) ;
#19505 = EDGE_LOOP ( 'NONE', ( #23412, #13560, #21077, #21606 ) ) ;
#19506 = CARTESIAN_POINT ( 'NONE',  ( 0.000000000000000000, 0.000000000000000000, 0.000000000000000000 ) ) ;
#19507 = ORIENTED_EDGE ( 'NONE', *, *, #551, .F. ) ;
#19508 = LINE ( 'NONE', #951, #21653 ) ;
#19509 = DIRECTION ( 'NONE',  ( -0.9892101392001054760, 0.1465035852930155480, 4.472400123700476920E-12 ) ) ;
#19510 = EDGE_LOOP ( 'NONE', ( #1729, #10485, #13751, #13061 ) ) ;
#19511 = DIRECTION ( 'NONE',  ( 2.507771768020000122E-12, -0.000000000000000000, -1.000000000000000000 ) ) ;
#19512 =( BOUNDED_CURVE ( )  B_SPLINE_CURVE ( 5, ( #329, #20326, #4019, #11247, #2240, #9461 ),
 .UNSPECIFIED., .F., .F. ) 
 B_SPLINE_CURVE_WITH_KNOTS ( ( 6, 6 ),
 ( 0.000000000000000000, 1.570796326712887714 ),
 .UNSPECIFIED. ) 
 CURVE ( )  GEOMETRIC_REPRESENTATION_ITEM ( )  RATIONAL_B_SPLINE_CURVE ( ( 1.000000000000000000, 0.6000000000209096962, 0.4000000000209096296, 0.3000000000156822222, 0.2500000000104548037, 0.2499999999999999445 ) ) 
 REPRESENTATION_ITEM ( '' )  );
#19513 = DIRECTION ( 'NONE',  ( -1.000000000000000000, 0.000000000000000000, 2.257221436789999912E-12 ) ) ;
#19514 = CARTESIAN_POINT ( 'NONE',  ( -24.26662447749999885, 35.20109951629999756, -148.0073960930000112 ) ) ;
#19515 = ADVANCED_FACE ( 'NONE', ( #4188 ), #265, .F. ) ;
#19516 = CONICAL_SURFACE ( 'NONE', #6422, 1.999999999999992450, 0.7853981633970000820 ) ;
#19517 = ADVANCED_FACE ( 'NONE', ( #11299 ), #13211, .F. ) ;
#19518 = ORIENTED_EDGE ( 'NONE', *, *, #11166, .T. ) ;
#19519 = CARTESIAN_POINT ( 'NONE',  ( -34.50000000000000000, 47.00000000000000000, -141.5552959529999839 ) ) ;
#19520 = PLANE ( 'NONE',  #23374 ) ;
#19521 = CARTESIAN_POINT ( 'NONE',  ( -14.84561440075239780, 36.91926241633263572, -147.9647079511389620 ) ) ;
#19522 = CARTESIAN_POINT ( 'NONE',  ( -28.59509960825648278, 39.22088873720170454, -140.4143345430010470 ) ) ;
#19523 = ORIENTED_EDGE ( 'NONE', *, *, #10388, .T. ) ;
#19524 = LINE ( 'NONE', #21790, #2582 ) ;
#19525 = DIRECTION ( 'NONE',  ( 1.000000000000000000, 0.000000000000000000, -2.259525899719999991E-12 ) ) ;
#19526 = LINE ( 'NONE', #8665, #12912 ) ;
#19527 = CARTESIAN_POINT ( 'NONE',  ( 32.50000000000000000, 39.80430157320000006, -149.5552959529999839 ) ) ;
#19528 = CARTESIAN_POINT ( 'NONE',  ( -24.10813950047970522, 36.95059904179322530, -147.5089432696624954 ) ) ;
#19529 = LINE ( 'NONE', #15829, #19326 ) ;
#19530 = VERTEX_POINT ( 'NONE', #14774 ) ;
#19531 = PLANE ( 'NONE',  #3486 ) ;
#19532 = LINE ( 'NONE', #8800, #6485 ) ;
#19533 = CARTESIAN_POINT ( 'NONE',  ( -32.50000000000000000, -50.00000000000000000, -137.0552959530000123 ) ) ;
#19534 = CARTESIAN_POINT ( 'NONE',  ( -8.594304764359998572, -10.75357442870000035, -145.5552959529999839 ) ) ;
#19535 = DIRECTION ( 'NONE',  ( 1.000000000000000000, 0.000000000000000000, 0.000000000000000000 ) ) ;
#19536 = CARTESIAN_POINT ( 'NONE',  ( -31.75000000000000000, -51.50000000000000000, -149.5552959529999839 ) ) ;
#19537 = EDGE_CURVE ( 'NONE', #712, #19545, #5841, .T. ) ;
#19538 = ORIENTED_EDGE ( 'NONE', *, *, #18801, .F. ) ;
#19539 = AXIS2_PLACEMENT_3D ( 'NONE', #18904, #9966, #11874 ) ;
#19540 = PLANE ( 'NONE',  #16828 ) ;
#19541 = DIRECTION ( 'NONE',  ( 2.602084747549999882E-17, -1.000000000000000000, -5.873289694040000105E-29 ) ) ;
#19542 = EDGE_LOOP ( 'NONE', ( #10662, #913, #5481, #18756, #5576, #10424, #4014, #7323 ) ) ;
#19543 = FACE_OUTER_BOUND ( 'NONE', #15355, .T. ) ;
#19544 = CARTESIAN_POINT ( 'NONE',  ( 16.65421564080000039, -18.61497348660000029, -145.5552959529999839 ) ) ;
#19545 = VERTEX_POINT ( 'NONE', #16905 ) ;
#19546 = CARTESIAN_POINT ( 'NONE',  ( -32.50000000000000000, 50.00000000000000000, -149.5552959529999839 ) ) ;
#19547 = CARTESIAN_POINT ( 'NONE',  ( 6.477506801250000557, -13.91317765220000169, -147.5552959529999839 ) ) ;
#19548 = CARTESIAN_POINT ( 'NONE',  ( -15.50000000000000000, 47.50000000000000000, -137.0552959530000123 ) ) ;
#19549 = CARTESIAN_POINT ( 'NONE',  ( 7.098883623607016524, 36.46423812985609203, -141.6133621761054826 ) ) ;
#19550 = VERTEX_POINT ( 'NONE', #15005 ) ;
#19551 = CARTESIAN_POINT ( 'NONE',  ( -9.319507568709141765, 35.96837468366262414, -148.5620496009611884 ) ) ;
#19552 = CARTESIAN_POINT ( 'NONE',  ( 3.175121949262585286, 27.24084097722915132, -150.0552959529999839 ) ) ;
#19553 = CARTESIAN_POINT ( 'NONE',  ( -8.314736843700092805, 40.56062062648400257, -143.6903644850042099 ) ) ;
#19554 = CARTESIAN_POINT ( 'NONE',  ( 7.053444247358170216, -30.74994780906165204, -136.0552959530158716 ) ) ;
#19555 = VECTOR ( 'NONE', #4316, 1000.000000000000000 ) ;
#19556 = EDGE_CURVE ( 'NONE', #11683, #4666, #15248, .T. ) ;
#19557 = ORIENTED_EDGE ( 'NONE', *, *, #5568, .F. ) ;
#19558 = CARTESIAN_POINT ( 'NONE',  ( -21.12031522135587380, 37.91567797510568028, -148.6783548734256328 ) ) ;
#19559 = ORIENTED_EDGE ( 'NONE', *, *, #12358, .T. ) ;
#19560 = CARTESIAN_POINT ( 'NONE',  ( -7.811725169189109863, 33.27862147039694207, -143.8116909731542705 ) ) ;
#19561 = CARTESIAN_POINT ( 'NONE',  ( -5.762834417829999722, 39.50865942520000118, -140.4825946859999988 ) ) ;
#19562 = DIRECTION ( 'NONE',  ( 0.000000000000000000, 1.000000000000000000, 0.000000000000000000 ) ) ;
#19563 = EDGE_CURVE ( 'NONE', #9566, #12161, #6199, .T. ) ;
#19564 = ORIENTED_EDGE ( 'NONE', *, *, #6593, .T. ) ;
#19565 = FACE_OUTER_BOUND ( 'NONE', #11586, .T. ) ;
#19566 = CARTESIAN_POINT ( 'NONE',  ( -6.270646159103367978, -16.71437421844448323, -146.5552959529736654 ) ) ;
#19567 = EDGE_CURVE ( 'NONE', #14976, #2513, #13334, .T. ) ;
#19568 = ORIENTED_EDGE ( 'NONE', *, *, #12733, .F. ) ;
#19569 = CARTESIAN_POINT ( 'NONE',  ( 1.133692148550000001, 51.50000000000000000, -136.5552959530000123 ) ) ;
#19570 = EDGE_CURVE ( 'NONE', #10546, #15560, #3953, .T. ) ;
#19571 = EDGE_CURVE ( 'NONE', #8129, #17769, #20486, .T. ) ;
#19572 = FACE_OUTER_BOUND ( 'NONE', #20079, .T. ) ;
#19573 = CARTESIAN_POINT ( 'NONE',  ( 16.33424841169999908, -31.58611763329999889, -147.5552959529999839 ) ) ;
#19574 = CARTESIAN_POINT ( 'NONE',  ( -12.76385253890000016, 37.02886902030000016, -147.6186336929999925 ) ) ;
#19575 = CARTESIAN_POINT ( 'NONE',  ( 10.68320006080000084, -21.50000000000000000, -150.0552959529999839 ) ) ;
#19576 = DIRECTION ( 'NONE',  ( -0.9840552701943220404, 0.1778629393740580045, -3.541738516501160129E-14 ) ) ;
#19577 = ITEM_DEFINED_TRANSFORMATION ( 'NONE', 'NONE', #3552,  #5025 ) ;
#19578 = DIRECTION ( 'NONE',  ( 0.000000000000000000, 1.000000000000000000, 0.000000000000000000 ) ) ;
#19579 = LINE ( 'NONE', #23147, #11191 ) ;
#19580 = ORIENTED_EDGE ( 'NONE', *, *, #13206, .T. ) ;
#19581 = CARTESIAN_POINT ( 'NONE',  ( -22.56584646716593667, 37.05444931714164625, -139.6092474954592433 ) ) ;
#19582 = ORIENTED_EDGE ( 'NONE', *, *, #17136, .F. ) ;
#19583 =( NAMED_UNIT ( * ) SI_UNIT ( $, .STERADIAN. ) SOLID_ANGLE_UNIT ( ) );
#19584 = MANIFOLD_SOLID_BREP ( 'lock_assembly.1\\lock body face plate inner.1\\PartBody', #7286 ) ;
#19585 = ORIENTED_EDGE ( 'NONE', *, *, #13310, .F. ) ;
#19586 = AXIS2_PLACEMENT_3D ( 'NONE', #15767, #8726, #10628 ) ;
#19587 = LINE ( 'NONE', #21495, #15593 ) ;
#19588 = CARTESIAN_POINT ( 'NONE',  ( -28.28132655699793929, 35.56853653578105678, -140.6131719533408102 ) ) ;
#19589 = VERTEX_POINT ( 'NONE', #22974 ) ;
#19590 = EDGE_CURVE ( 'NONE', #21465, #20697, #2174, .T. ) ;
#19591 = VERTEX_POINT ( 'NONE', #17261 ) ;
#19592 = CARTESIAN_POINT ( 'NONE',  ( -7.101996734231647679, 19.50000000000000711, -150.0552959529999839 ) ) ;
#19593 = CARTESIAN_POINT ( 'NONE',  ( -9.674592407259998694, 39.37273218290000187, -147.1879168910000146 ) ) ;
#19594 = ADVANCED_FACE ( 'NONE', ( #17617 ), #6776, .T. ) ;
#19595 = CARTESIAN_POINT ( 'NONE',  ( -11.32406291796261399, 40.56182626977977179, -143.8345514045001892 ) ) ;
#19596 = DIRECTION ( 'NONE',  ( -1.000000000000000000, 0.000000000000000000, 2.257171095940000041E-12 ) ) ;
#19597 = DIRECTION ( 'NONE',  ( -1.000000000000000000, 0.000000000000000000, -2.245315044999999693E-12 ) ) ;
#19598 = ORIENTED_EDGE ( 'NONE', *, *, #8404, .T. ) ;
#19599 = CARTESIAN_POINT ( 'NONE',  ( 9.225170223517482171, 35.68671641322836052, -141.9279471768529390 ) ) ;
#19600 = CYLINDRICAL_SURFACE ( 'NONE', #4166, 7.500000000000006217 ) ;
#19601 = AXIS2_PLACEMENT_3D ( 'NONE', #12278, #23002, #4916 ) ;
#19602 = CARTESIAN_POINT ( 'NONE',  ( -5.758148842630000708, -13.22138763369999914, -147.5552959529999839 ) ) ;
#19603 = AXIS2_PLACEMENT_3D ( 'NONE', #8016, #11823, #22664 ) ;
#19604 = ORIENTED_EDGE ( 'NONE', *, *, #10061, .F. ) ;
#19605 = LINE ( 'NONE', #17940, #12947 ) ;
#19606 = ORIENTED_EDGE ( 'NONE', *, *, #6146, .F. ) ;
#19607 = CARTESIAN_POINT ( 'NONE',  ( -32.99999999989999822, 37.00000000000000000, -138.5552959529999839 ) ) ;
#19608 = CARTESIAN_POINT ( 'NONE',  ( 5.276897646260000130, -21.39828525539999760, -144.5552959529999839 ) ) ;
#19609 = ORIENTED_EDGE ( 'NONE', *, *, #21019, .F. ) ;
#19610 = CARTESIAN_POINT ( 'NONE',  ( -19.92532084500992440, 37.01154022404042365, -139.3892291660651779 ) ) ;
#19611 = DIRECTION ( 'NONE',  ( 1.000000000000000000, 0.000000000000000000, 0.000000000000000000 ) ) ;
#19612 = EDGE_LOOP ( 'NONE', ( #19398, #8426 ) ) ;
#19613 = CARTESIAN_POINT ( 'NONE',  ( -15.90674982584208941, 37.04592612750104053, -148.5146100863323966 ) ) ;
#19614 = LINE ( 'NONE', #21409, #4568 ) ;
#19615 = ORIENTED_EDGE ( 'NONE', *, *, #16910, .T. ) ;
#19616 = EDGE_CURVE ( 'NONE', #7320, #22094, #7874, .T. ) ;
#19617 = ORIENTED_EDGE ( 'NONE', *, *, #3801, .T. ) ;
#19618 = DIRECTION ( 'NONE',  ( -2.688820921349999492E-17, 1.000000000000000000, 6.069065783950000909E-29 ) ) ;
#19619 = EDGE_CURVE ( 'NONE', #12394, #9978, #6546, .T. ) ;
#19620 = CIRCLE ( 'NONE', #7061, 2.500000000000002220 ) ;
#19621 = FACE_OUTER_BOUND ( 'NONE', #11493, .T. ) ;
#19622 = VERTEX_POINT ( 'NONE', #15470 ) ;
#19623 = CARTESIAN_POINT ( 'NONE',  ( -2.499999999969999998, 40.00000000000000000, -137.0552959530000123 ) ) ;
#19624 = CARTESIAN_POINT ( 'NONE',  ( 2.170391987449999505, -12.72823260819999902, -146.5552959529999839 ) ) ;
#19625 = ORIENTED_EDGE ( 'NONE', *, *, #3520, .F. ) ;
#19626 = CARTESIAN_POINT ( 'NONE',  ( -13.47165290130000059, 33.35876621949999787, -143.8174469059999865 ) ) ;
#19627 = ORIENTED_EDGE ( 'NONE', *, *, #16238, .F. ) ;
#19628 = PLANE ( 'NONE',  #14703 ) ;
#19629 = LINE ( 'NONE', #1915, #18815 ) ;
#19630 = CARTESIAN_POINT ( 'NONE',  ( -14.97130487713839919, 37.69282299035099015, -147.6145025267201447 ) ) ;
#19631 = LINE ( 'NONE', #16182, #9839 ) ;
#19632 = CIRCLE ( 'NONE', #23051, 5.999999999999998224 ) ;
#19633 = ORIENTED_EDGE ( 'NONE', *, *, #2702, .F. ) ;
#19634 = CARTESIAN_POINT ( 'NONE',  ( 4.553999924799793320, 13.23986818282720890, -136.0552959530102726 ) ) ;
#19635 = LINE ( 'NONE', #1571, #3652 ) ;
#19636 = DIRECTION ( 'NONE',  ( -0.9919007982877544594, 0.1270149847699686418, 4.677746543438841512E-14 ) ) ;
#19637 = DIRECTION ( 'NONE',  ( 0.06298685227120542907, 0.9980143568310855251, -1.492139745100128694E-13 ) ) ;
#19638 = LINE ( 'NONE', #10694, #15270 ) ;
#19639 = CARTESIAN_POINT ( 'NONE',  ( 2.139623390130000136, -12.81320239329999922, -144.5552959529999839 ) ) ;
#19640 = ORIENTED_EDGE ( 'NONE', *, *, #6753, .T. ) ;
#19641 = CARTESIAN_POINT ( 'NONE',  ( 7.750000000030000002, -38.98606797749999942, -137.0552959530000123 ) ) ;
#19642 = DIRECTION ( 'NONE',  ( 0.000000000000000000, -1.000000000000000000, 0.000000000000000000 ) ) ;
#19643 = EDGE_CURVE ( 'NONE', #16248, #22660, #15500, .T. ) ;
#19644 = DIRECTION ( 'NONE',  ( -0.6459422414661291079, 0.7633862853691523176, -2.273736754430455399E-12 ) ) ;
#19645 = CARTESIAN_POINT ( 'NONE',  ( -6.807579269548480028, 38.78453684422532177, -147.8970667729606134 ) ) ;
#19646 = CARTESIAN_POINT ( 'NONE',  ( -24.68730002459999895, 39.33688142210000649, -147.2285014869999884 ) ) ;
#19647 = EDGE_CURVE ( 'NONE', #8811, #1347, #15870, .T. ) ;
#19648 = DIRECTION ( 'NONE',  ( 0.1736481776649230202, 0.000000000000000000, -0.9848077530125619594 ) ) ;
#19649 = AXIS2_PLACEMENT_3D ( 'NONE', #12771, #20045, #14681 ) ;
#19650 = ORIENTED_EDGE ( 'NONE', *, *, #23539, .F. ) ;
#19651 = CARTESIAN_POINT ( 'NONE',  ( 0.000000000000000000, 0.000000000000000000, -150.0552959529999839 ) ) ;
#19652 = AXIS2_PLACEMENT_3D ( 'NONE', #13619, #19465, #2805 ) ;
#19653 = CARTESIAN_POINT ( 'NONE',  ( 5.700764968559962398, -2.580208454387413752, -150.0552959529999839 ) ) ;
#19654 = VERTEX_POINT ( 'NONE', #20833 ) ;
#19655 = PRODUCT ( 'Lock Tumblers', 'Lock Tumblers', '', ( #3784 ) ) ;
#19656 = CARTESIAN_POINT ( 'NONE',  ( -6.601136089949999786, -20.10368962670000315, -143.5552959529999839 ) ) ;
#19657 = ORIENTED_EDGE ( 'NONE', *, *, #12977, .T. ) ;
#19658 = DIRECTION ( 'NONE',  ( 8.954614827420000395E-12, -9.094947017729999296E-13, 1.000000000000000000 ) ) ;
#19659 = LINE ( 'NONE', #19547, #11996 ) ;
#19660 = DIRECTION ( 'NONE',  ( -0.09606172499277226828, -0.9953753789357124848, 8.268133652477615271E-13 ) ) ;
#19661 = CARTESIAN_POINT ( 'NONE',  ( 7.108347771513900071, 36.44011433609385620, -141.6187646495017702 ) ) ;
#19662 = ORIENTED_EDGE ( 'NONE', *, *, #2649, .T. ) ;
#19663 = CARTESIAN_POINT ( 'NONE',  ( -18.18930989808823995, 36.96028804432864234, -147.6841622078175931 ) ) ;
#19664 = AXIS2_PLACEMENT_3D ( 'NONE', #4269, #16757, #7707 ) ;
#19665 = CARTESIAN_POINT ( 'NONE',  ( -7.499999999959999997, 22.50000000000000000, -136.0552959530000123 ) ) ;
#19666 = CARTESIAN_POINT ( 'NONE',  ( 9.736704675149560728, -34.16257638424990972, -136.0552959530219823 ) ) ;
#19667 = ORIENTED_EDGE ( 'NONE', *, *, #15168, .F. ) ;
#19668 = STYLED_ITEM ( 'NONE', ( #20604 ), #19475 ) ;
#19669 = CARTESIAN_POINT ( 'NONE',  ( 15.50000000000000000, 36.50000000000000000, -150.0552959529999839 ) ) ;
#19670 = ORIENTED_EDGE ( 'NONE', *, *, #6340, .T. ) ;
#19671 = DIRECTION ( 'NONE',  ( 2.257144641399999941E-12, -8.049597179213198935E-35, 1.000000000000000000 ) ) ;
#19672 = CARTESIAN_POINT ( 'NONE',  ( -5.972224716009999490, 40.79464204750000533, -141.7656025439999894 ) ) ;
#19673 = EDGE_CURVE ( 'NONE', #9183, #3527, #17912, .T. ) ;
#19674 = LINE ( 'NONE', #7406, #6614 ) ;
#19675 = ORIENTED_EDGE ( 'NONE', *, *, #14903, .T. ) ;
#19676 = CARTESIAN_POINT ( 'NONE',  ( 21.39890631740000160, -21.26106171180000359, -144.5552959529999839 ) ) ;
#19677 = CARTESIAN_POINT ( 'NONE',  ( 24.87050155979999744, -26.86223000240000047, -145.5552959529999839 ) ) ;
#19678 = ORIENTED_EDGE ( 'NONE', *, *, #10355, .T. ) ;
#19679 = CARTESIAN_POINT ( 'NONE',  ( -9.347107914279998653, -17.32706600430000066, -143.5552959529999839 ) ) ;
#19680 = VECTOR ( 'NONE', #16127, 1000.000000000000000 ) ;
#19681 = EDGE_CURVE ( 'NONE', #2494, #5644, #13923, .T. ) ;
#19682 = CARTESIAN_POINT ( 'NONE',  ( 17.57628698940784773, 21.71923945896039854, -150.0552959529999839 ) ) ;
#19683 = CARTESIAN_POINT ( 'NONE',  ( -18.00000000000000000, -43.00000000000000000, -150.0552959529999839 ) ) ;
#19684 = DIRECTION ( 'NONE',  ( 2.507771768019999718E-12, 1.592654864209999947E-17, -1.000000000000000000 ) ) ;
#19685 = CARTESIAN_POINT ( 'NONE',  ( -34.61111111099999960, 26.50000000000000000, -140.5552959529999839 ) ) ;
#19686 = FACE_OUTER_BOUND ( 'NONE', #2291, .T. ) ;
#19687 = CONTEXT_DEPENDENT_SHAPE_REPRESENTATION ( #21664, #11807 ) ;
#19688 = LINE ( 'NONE', #21952, #19250 ) ;
#19689 = PLANE ( 'NONE',  #961 ) ;
#19690 = ADVANCED_FACE ( 'NONE', ( #20714 ), #12127, .T. ) ;
#19691 = CARTESIAN_POINT ( 'NONE',  ( 18.95053822279999878, -51.50000000000000000, -149.5552959529999839 ) ) ;
#19692 = ORIENTED_EDGE ( 'NONE', *, *, #6481, .T. ) ;
#19693 = UNCERTAINTY_MEASURE_WITH_UNIT (LENGTH_MEASURE( 1.000000000000000082E-05 ), #14228, 'distance_accuracy_value', 'NONE');
#19694 = EDGE_CURVE ( 'NONE', #8186, #23343, #23089, .T. ) ;
#19696 = VERTEX_POINT ( 'NONE', #11768 ) ;
#19695 = VECTOR ( 'NONE', #6072, 1000.000000000000000 ) ;
#19697 = SURFACE_SIDE_STYLE ('',( #16132 ) ) ;
#19698 = COLOUR_RGB ( '', 0.09019608, 0.27058824, 0.51372549) ;
#19699 = ORIENTED_EDGE ( 'NONE', *, *, #13973, .T. ) ;
#19700 = LINE ( 'NONE', #10872, #402 ) ;
#19701 = CARTESIAN_POINT ( 'NONE',  ( -27.83857872746931506, 33.37060406817593616, -143.5613806138642872 ) ) ;
#19702 = VERTEX_POINT ( 'NONE', #17142 ) ;
#19703 = EDGE_CURVE ( 'NONE', #17877, #6526, #17373, .T. ) ;
#19704 = LINE ( 'NONE', #10639, #1308 ) ;
#19705 = VERTEX_POINT ( 'NONE', #8090 ) ;
#19706 = CARTESIAN_POINT ( 'NONE',  ( 24.33939095838566047, 38.90181682662307594, -136.0552959530549515 ) ) ;
#19707 = CARTESIAN_POINT ( 'NONE',  ( -19.58896675450998615, 35.53469097119599240, -140.8466141450865621 ) ) ;
#19708 = CARTESIAN_POINT ( 'NONE',  ( -11.19078917913330962, 40.90943599255746932, -144.6700718817450593 ) ) ;
#19709 = LINE ( 'NONE', #8977, #2705 ) ;
#19710 = ORIENTED_EDGE ( 'NONE', *, *, #2189, .F. ) ;
#19711 = DIRECTION ( 'NONE',  ( 1.000000000000000000, 0.000000000000000000, 0.000000000000000000 ) ) ;
#19712 = EDGE_LOOP ( 'NONE', ( #20870, #16389, #10107, #4016, #10967 ) ) ;
#19713 = EDGE_CURVE ( 'NONE', #7623, #8661, #22166, .T. ) ;
#19714 = CARTESIAN_POINT ( 'NONE',  ( 9.161058160660402905, 35.65265274061410139, -141.9492515423469285 ) ) ;
#19715 = ADVANCED_FACE ( 'NONE', ( #131 ), #12826, .T. ) ;
#19716 = DIRECTION ( 'NONE',  ( 0.000000000000000000, 1.000000000000000000, -2.245315044999999693E-12 ) ) ;
#19717 = CIRCLE ( 'NONE', #20482, 2.000000000000000000 ) ;
#19718 = LINE ( 'NONE', #10887, #7216 ) ;
#19719 = ORIENTED_EDGE ( 'NONE', *, *, #13432, .F. ) ;
#19720 = VECTOR ( 'NONE', #5905, 1000.000000000000000 ) ;
#19721 = EDGE_CURVE ( 'NONE', #22142, #16387, #19524, .T. ) ;
#19722 = VECTOR ( 'NONE', #16408, 1000.000000000000000 ) ;
#19723 = EDGE_CURVE ( 'NONE', #7689, #4619, #3329, .T. ) ;
#19724 = DIRECTION ( 'NONE',  ( 2.507771768020000122E-12, -0.000000000000000000, -1.000000000000000000 ) ) ;
#19725 = ORIENTED_EDGE ( 'NONE', *, *, #10934, .F. ) ;
#19726 = CARTESIAN_POINT ( 'NONE',  ( -19.59255166829999695, 37.05126161860000167, -140.3061871179999969 ) ) ;
#19727 = CARTESIAN_POINT ( 'NONE',  ( -5.499999999969999109, 44.50000000000000000, -136.5552959530000123 ) ) ;
#19728 = ADVANCED_FACE ( 'NONE', ( #7134 ), #8, .T. ) ;
#19729 = EDGE_LOOP ( 'NONE', ( #7361, #10928, #18924, #2721, #7021, #4847, #10910, #7609, #20353, #6308, #14234, #8466 ) ) ;
#19730 = CARTESIAN_POINT ( 'NONE',  ( 9.183200060760000838, -21.50000000000000000, -148.5552959529999839 ) ) ;
#19731 = ADVANCED_BREP_SHAPE_REPRESENTATION ( '', ( #19431, #5025 ), #3911 ) ;
#19732 = ORIENTED_EDGE ( 'NONE', *, *, #19813, .T. ) ;
#19733 = CARTESIAN_POINT ( 'NONE',  ( -15.17828643423089829, 39.13746915041124197, -146.9793796816295810 ) ) ;
#19734 = EDGE_CURVE ( 'NONE', #19705, #2700, #14524, .T. ) ;
#19735 = CARTESIAN_POINT ( 'NONE',  ( 2.508811538190000245, -14.35090895149999923, -145.5552959529999839 ) ) ;
#19736 = VERTEX_POINT ( 'NONE', #14394 ) ;
#19737 =( LENGTH_UNIT ( ) NAMED_UNIT ( * ) SI_UNIT ( .MILLI., .METRE. ) );
#19738 = AXIS2_PLACEMENT_3D ( 'NONE', #19544, #15842, #22885 ) ;
#19739 = ORIENTED_EDGE ( 'NONE', *, *, #5055, .F. ) ;
#19740 = FACE_OUTER_BOUND ( 'NONE', #16253, .T. ) ;
#19741 = VECTOR ( 'NONE', #14371, 1000.000000000000000 ) ;
#19742 = CARTESIAN_POINT ( 'NONE',  ( 13.13369214870000157, -51.50000000000000000, -136.5552959530000123 ) ) ;
#19743 = VERTEX_POINT ( 'NONE', #10690 ) ;
#19744 = PLANE ( 'NONE',  #7223 ) ;
#19745 = VECTOR ( 'NONE', #19644, 1000.000000000000227 ) ;
#19746 = CARTESIAN_POINT ( 'NONE',  ( -10.84486070616090991, 35.03979930411003352, -141.1912331422082900 ) ) ;
#19747 = VECTOR ( 'NONE', #16750, 1000.000000000000000 ) ;
#19748 = DIRECTION ( 'NONE',  ( 0.000000000000000000, -1.000000000000000000, 0.000000000000000000 ) ) ;
#19749 = ORIENTED_EDGE ( 'NONE', *, *, #16953, .T. ) ;
#19750 = MANIFOLD_SOLID_BREP ( 'lock_assembly.1\\Part1.2\\PartBody', #6887 ) ;
#19751 = CARTESIAN_POINT ( 'NONE',  ( -12.50000000000000000, -2.273736754430000208E-12, -136.0552959530000123 ) ) ;
#19752 = ORIENTED_EDGE ( 'NONE', *, *, #16126, .T. ) ;
#19753 = DIRECTION ( 'NONE',  ( 2.257171095940000041E-12, 1.003664318210000046E-28, 1.000000000000000000 ) ) ;
#19754 = VECTOR ( 'NONE', #1298, 1000.000000000000000 ) ;
#19755 = AXIS2_PLACEMENT_3D ( 'NONE', #21543, #3571, #10563 ) ;
#19756 = EDGE_CURVE ( 'NONE', #11584, #7053, #3455, .T. ) ;
#19757 = CARTESIAN_POINT ( 'NONE',  ( -14.12939694657403678, 41.07986042234944080, -141.7257002008347229 ) ) ;
#19758 = CARTESIAN_POINT ( 'NONE',  ( -28.79441775903490353, 39.40253724237003041, -140.0594529943023758 ) ) ;
#19759 = ORIENTED_EDGE ( 'NONE', *, *, #7611, .F. ) ;
#19760 = CARTESIAN_POINT ( 'NONE',  ( -26.47299999999999898, 14.00000000000000000, -144.0552959529999839 ) ) ;
#19761 = CARTESIAN_POINT ( 'NONE',  ( -2.100773033209999863, -15.22510554480000167, -146.5552959529999839 ) ) ;
#19762 = CIRCLE ( 'NONE', #23167, 0.7500000000000006661 ) ;
#19763 = LINE ( 'NONE', #133, #22432 ) ;
#19764 = FACE_OUTER_BOUND ( 'NONE', #20059, .T. ) ;
#19765 = CARTESIAN_POINT ( 'NONE',  ( -24.06602356359999817, 36.94557182220000158, -148.2530914610000252 ) ) ;
#19766 = VECTOR ( 'NONE', #1060, 1000.000000000000000 ) ;
#19767 = DIRECTION ( 'NONE',  ( 0.000000000000000000, 0.000000000000000000, 1.000000000000000000 ) ) ;
#19768 = ORIENTED_EDGE ( 'NONE', *, *, #19619, .T. ) ;
#19769 = DIRECTION ( 'NONE',  ( -1.000000000000000000, -2.602084704489999637E-17, 1.701177084830000066E-20 ) ) ;
#19770 = B_SPLINE_CURVE_WITH_KNOTS ( 'NONE', 3,
 ( #5484, #5367, #1579, #1933, #5594, #18097, #21912, #12728, #250, #12843, #10702, #21556, #5238, #23, #19772, #1807, #7382, #5711 ),
 .UNSPECIFIED., .F., .F.,
 ( 4, 2, 2, 2, 2, 2, 2, 2, 4 ),
 ( 0.000000000000000000, 0.1250000000000000000, 0.2500000000000000000, 0.3750000000000000000, 0.5000000000000000000, 0.6250000000000000000, 0.7500000000000000000, 0.8750000000000000000, 1.000000000000000000 ),
 .UNSPECIFIED. ) ;
#19771 = FACE_BOUND ( 'NONE', #19344, .T. ) ;
#19772 = CARTESIAN_POINT ( 'NONE',  ( 7.121359165062779439, -5.010856941112688645, -150.0552959529999839 ) ) ;
#19773 = FACE_OUTER_BOUND ( 'NONE', #2775, .T. ) ;
#19774 = DIRECTION ( 'NONE',  ( 2.257144641397284947E-12, -2.714724913984255017E-24, 1.000000000000000000 ) ) ;
#19775 = ORIENTED_EDGE ( 'NONE', *, *, #22788, .F. ) ;
#19776 = FACE_OUTER_BOUND ( 'NONE', #22721, .T. ) ;
#19777 = CARTESIAN_POINT ( 'NONE',  ( 19.77963439019999825, 51.26338628519999929, -143.0552959529999839 ) ) ;
#19778 = ORIENTED_EDGE ( 'NONE', *, *, #4558, .T. ) ;
#19779 = CIRCLE ( 'NONE', #22418, 14.99999999999999822 ) ;
#19780 = VECTOR ( 'NONE', #22904, 1000.000000000000000 ) ;
#19781 = VECTOR ( 'NONE', #805, 1000.000000000000000 ) ;
#19782 = FACE_OUTER_BOUND ( 'NONE', #13642, .T. ) ;
#19783 = VERTEX_POINT ( 'NONE', #1796 ) ;
#19784 = CARTESIAN_POINT ( 'NONE',  ( 4.750000000000000000, -38.23606797749999942, -150.5552959529999839 ) ) ;
#19785 = EDGE_CURVE ( 'NONE', #7205, #915, #1453, .T. ) ;
#19786 = CARTESIAN_POINT ( 'NONE',  ( -30.05504742970118670, 39.87093548741106019, -141.1846073849872312 ) ) ;
#19787 = DIRECTION ( 'NONE',  ( 1.000000000000000000, 0.000000000000000000, -4.511206223393553012E-12 ) ) ;
#19788 = CARTESIAN_POINT ( 'NONE',  ( 7.151459560400827087, 37.65757145640934311, -141.6431750412416193 ) ) ;
#19789 = ORIENTED_EDGE ( 'NONE', *, *, #4226, .T. ) ;
#19790 = CARTESIAN_POINT ( 'NONE',  ( -10.56415788819999868, 36.18163687389999694, -139.7056672729999889 ) ) ;
#19791 = EDGE_CURVE ( 'NONE', #17461, #15193, #12450, .T. ) ;
#19792 = CARTESIAN_POINT ( 'NONE',  ( -18.56307309666442862, 32.92303375952681677, -144.6176528170184099 ) ) ;
#19793 = CARTESIAN_POINT ( 'NONE',  ( -8.831009117212259341, 37.75574244304178961, -147.9814132533029465 ) ) ;
#19794 = CARTESIAN_POINT ( 'NONE',  ( 4.020454867604463800, -35.03105831636347745, -136.0552959530090789 ) ) ;
#19795 = ORIENTED_EDGE ( 'NONE', *, *, #10262, .F. ) ;
#19796 = VECTOR ( 'NONE', #22012, 1000.000000000000000 ) ;
#19797 = VECTOR ( 'NONE', #8595, 1000.000000000000000 ) ;
#19798 = CARTESIAN_POINT ( 'NONE',  ( 20.10199673425611877, 25.50000000000003197, -136.0552959530453450 ) ) ;
#19799 = VERTEX_POINT ( 'NONE', #20342 ) ;
#19800 = CARTESIAN_POINT ( 'NONE',  ( -9.334216945200001447, -17.19633444960000190, -145.5552959529999839 ) ) ;
#19801 = CARTESIAN_POINT ( 'NONE',  ( -23.76507348470000025, 39.47303768190000284, -147.6024660349999920 ) ) ;
#19802 = CARTESIAN_POINT ( 'NONE',  ( -7.499999999959999997, 19.50000000000000000, -136.0552959530000123 ) ) ;
#19803 = ORIENTED_EDGE ( 'NONE', *, *, #3888, .F. ) ;
#19804 = DIRECTION ( 'NONE',  ( -0.9753087663813413410, 0.2208456705930775810, 0.000000000000000000 ) ) ;
#19805 = DIRECTION ( 'NONE',  ( -0.1000233216789610108, -0.9949850929136109245, 3.576398436658600095E-13 ) ) ;
#19806 = VERTEX_POINT ( 'NONE', #21900 ) ;
#19807 = CARTESIAN_POINT ( 'NONE',  ( -18.08788331839999941, 37.73304001160000354, -147.6923967950000076 ) ) ;
#19808 = FACE_OUTER_BOUND ( 'NONE', #18594, .T. ) ;
#19809 = CARTESIAN_POINT ( 'NONE',  ( -15.39054929727204879, -44.46182274717511973, -150.0552959529999839 ) ) ;
#19810 = AXIS2_PLACEMENT_3D ( 'NONE', #9684, #558, #21349 ) ;
#19811 = CARTESIAN_POINT ( 'NONE',  ( -15.00000000000000000, -41.50000000000000000, -136.0552959530000123 ) ) ;
#19812 = AXIS2_PLACEMENT_3D ( 'NONE', #10603, #16338, #1719 ) ;
#19813 = EDGE_CURVE ( 'NONE', #11004, #18991, #9604, .T. ) ;
#19814 = CARTESIAN_POINT ( 'NONE',  ( 31.50000000000000000, 20.96379895120000114, -136.0552959530000123 ) ) ;
#19815 = FACE_OUTER_BOUND ( 'NONE', #23398, .T. ) ;
#19816 = PLANE ( 'NONE',  #17760 ) ;
#19817 = EDGE_CURVE ( 'NONE', #17914, #384, #18535, .T. ) ;
#19818 = CARTESIAN_POINT ( 'NONE',  ( -9.334216945200001447, -17.19633444960000190, -146.5552959529999839 ) ) ;
#19819 = DIRECTION ( 'NONE',  ( -2.257157423930000049E-12, 0.000000000000000000, -1.000000000000000000 ) ) ;
#19820 = ORIENTED_EDGE ( 'NONE', *, *, #21534, .T. ) ;
#19821 = ORIENTED_EDGE ( 'NONE', *, *, #3997, .F. ) ;
#19822 = EDGE_LOOP ( 'NONE', ( #17220, #19609 ) ) ;
#19823 = DIRECTION ( 'NONE',  ( 0.000000000000000000, 1.000000000000000000, 0.000000000000000000 ) ) ;
#19824 = CARTESIAN_POINT ( 'NONE',  ( -33.50000000000000000, 46.00000000000000000, -141.5552959529999839 ) ) ;
#19825 = ORIENTED_EDGE ( 'NONE', *, *, #5030, .F. ) ;
#19826 = AXIS2_PLACEMENT_3D ( 'NONE', #1446, #8908, #23328 ) ;
#19827 = CARTESIAN_POINT ( 'NONE',  ( -25.35824191590000254, -34.50000000000000000, -145.5657682199999954 ) ) ;
#19828 = VECTOR ( 'NONE', #18095, 1000.000000000000000 ) ;
#19829 = ORIENTED_EDGE ( 'NONE', *, *, #4008, .F. ) ;
#19830 = PLANE ( 'NONE',  #19366 ) ;
#19831 = DIRECTION ( 'NONE',  ( -2.507771768019999718E-12, -1.592654864069999939E-17, 1.000000000000000000 ) ) ;
#19832 = CARTESIAN_POINT ( 'NONE',  ( -11.85909339607291457, 36.92087135288571886, -147.9691652862101421 ) ) ;
#19833 = DIRECTION ( 'NONE',  ( 0.1720749717299729364, 0.9850838563818457017, -6.484322019408987829E-13 ) ) ;
#19834 = VERTEX_POINT ( 'NONE', #5813 ) ;
#19835 = DIRECTION ( 'NONE',  ( 2.257144641399999941E-12, -8.049635416090000264E-35, 1.000000000000000000 ) ) ;
#19836 = EDGE_CURVE ( 'NONE', #18609, #22206, #7710, .T. ) ;
#19837 = ORIENTED_EDGE ( 'NONE', *, *, #1689, .F. ) ;
#19838 = CARTESIAN_POINT ( 'NONE',  ( 8.997695683344982598, 35.58457175570028852, -141.9945801902854328 ) ) ;
#19839 = DIRECTION ( 'NONE',  ( 2.257144641399999941E-12, -4.009147065140000298E-51, 1.000000000000000000 ) ) ;
#19840 = DIRECTION ( 'NONE',  ( 2.839308199620000013E-14, 3.568879590630000244E-13, 1.000000000000000000 ) ) ;
#19841 = STYLED_ITEM ( 'NONE', ( #4828 ), #16897 ) ;
#19842 = EDGE_CURVE ( 'NONE', #21873, #6393, #14977, .T. ) ;
#19843 = ORIENTED_EDGE ( 'NONE', *, *, #11522, .T. ) ;
#19844 = VECTOR ( 'NONE', #5993, 1000.000000000000000 ) ;
#19845 = AXIS2_PLACEMENT_3D ( 'NONE', #13824, #981, #21206 ) ;
#19846 = DIRECTION ( 'NONE',  ( 2.839308199593065147E-14, 3.568879590624614785E-13, 1.000000000000000000 ) ) ;
#19847 = VERTEX_POINT ( 'NONE', #2383 ) ;
#19848 = FACE_OUTER_BOUND ( 'NONE', #7063, .T. ) ;
#19849 = ORIENTED_EDGE ( 'NONE', *, *, #10863, .F. ) ;
#19850 = CARTESIAN_POINT ( 'NONE',  ( -10.49999999989999822, 34.50000000000000000, -144.0552959529999839 ) ) ;
#19851 = EDGE_LOOP ( 'NONE', ( #23338, #19353 ) ) ;
#19852 = CARTESIAN_POINT ( 'NONE',  ( -16.06083392305800928, 37.86731064063600627, -147.7990361411401068 ) ) ;
#19853 = EDGE_CURVE ( 'NONE', #4100, #18237, #2492, .T. ) ;
#19854 = CARTESIAN_POINT ( 'NONE',  ( -5.246523349656645685, 45.51000832343145674, -136.0552959529881605 ) ) ;
#19855 = ORIENTED_EDGE ( 'NONE', *, *, #6850, .F. ) ;
#19856 =( BOUNDED_CURVE ( )  B_SPLINE_CURVE ( 5, ( #14160, #12123, #15592, #11763, #2754, #23202 ),
 .UNSPECIFIED., .F., .F. ) 
 B_SPLINE_CURVE_WITH_KNOTS ( ( 6, 6 ),
 ( 0.000000000000000000, 1.570796326702242673 ),
 .UNSPECIFIED. ) 
 CURVE ( )  GEOMETRIC_REPRESENTATION_ITEM ( )  RATIONAL_B_SPLINE_CURVE ( ( 1.000000000000000000, 0.6000000000236205278, 0.4000000000236205167, 0.3000000000177153736, 0.2500000000118102750, 0.2500000000000000000 ) ) 
 REPRESENTATION_ITEM ( '' )  );
#19857 = ORIENTED_EDGE ( 'NONE', *, *, #7201, .F. ) ;
#19858 = CARTESIAN_POINT ( 'NONE',  ( -25.84964047037207990, 38.84307078610155628, -139.9757795274772150 ) ) ;
#19859 = FACE_OUTER_BOUND ( 'NONE', #16904, .T. ) ;
#19860 = EDGE_LOOP ( 'NONE', ( #609, #23520 ) ) ;
#19861 = DIRECTION ( 'NONE',  ( 0.1824094679249879947, 0.9832226533249336375, -8.292396948119437334E-13 ) ) ;
#19862 = VECTOR ( 'NONE', #13800, 1000.000000000000000 ) ;
#19863 = DIRECTION ( 'NONE',  ( -1.000000000000000000, 0.000000000000000000, 2.245315044999999693E-12 ) ) ;
#19864 = EDGE_CURVE ( 'NONE', #14150, #3155, #13303, .T. ) ;
#19865 = DIRECTION ( 'NONE',  ( 1.000000000000000000, 0.000000000000000000, 0.000000000000000000 ) ) ;
#19866 = VERTEX_POINT ( 'NONE', #5927 ) ;
#19867 = EDGE_CURVE ( 'NONE', #22408, #3155, #8190, .T. ) ;
#19868 = LINE ( 'NONE', #17962, #4523 ) ;
#19869 = EDGE_CURVE ( 'NONE', #11242, #21090, #1055, .T. ) ;
#19870 = ADVANCED_FACE ( 'NONE', ( #11502 ), #18781, .F. ) ;
#19871 = ORIENTED_EDGE ( 'NONE', *, *, #6911, .T. ) ;
#19872 = CARTESIAN_POINT ( 'NONE',  ( -4.500000000000000000, 40.00000000000000000, -151.0552959529999839 ) ) ;
#19873 = CARTESIAN_POINT ( 'NONE',  ( -10.88504013570612905, 37.01634837951200296, -139.4704149077907402 ) ) ;
#19874 = CARTESIAN_POINT ( 'NONE',  ( 14.79224200838147318, -1.499999999999999778, -141.9623572382618306 ) ) ;
#19875 = DIRECTION ( 'NONE',  ( 1.000000000000000000, 0.000000000000000000, -2.253752739989067373E-12 ) ) ;
#19876 = VERTEX_POINT ( 'NONE', #14632 ) ;
#19877 = DIRECTION ( 'NONE',  ( 0.000000000000000000, -1.000000000000000000, 0.000000000000000000 ) ) ;
#19878 = MECHANICAL_DESIGN_GEOMETRIC_PRESENTATION_REPRESENTATION (  '', ( #17210 ), #17598 ) ;
#19879 = CARTESIAN_POINT ( 'NONE',  ( 18.95053822279999878, 51.00000000000000000, -149.5552959529999839 ) ) ;
#19880 = VECTOR ( 'NONE', #1106, 1000.000000000000114 ) ;
#19881 = FACE_OUTER_BOUND ( 'NONE', #5821, .T. ) ;
#19882 = FACE_OUTER_BOUND ( 'NONE', #15206, .T. ) ;
#19883 = CARTESIAN_POINT ( 'NONE',  ( 31.96891336220000213, -40.94938100119999547, -149.8052959529999839 ) ) ;
#19884 = DIRECTION ( 'NONE',  ( 0.000000000000000000, 1.000000000000000000, 0.000000000000000000 ) ) ;
#19885 = ORIENTED_EDGE ( 'NONE', *, *, #513, .F. ) ;
#19886 = FACE_OUTER_BOUND ( 'NONE', #15734, .T. ) ;
#19887 = CARTESIAN_POINT ( 'NONE',  ( 14.50000000010000001, 37.00000000000000000, -144.0552959529999839 ) ) ;
#19888 = DIRECTION ( 'NONE',  ( 1.000000000000000000, 0.000000000000000000, 0.000000000000000000 ) ) ;
#19889 = CARTESIAN_POINT ( 'NONE',  ( -5.659867863851591352, 38.70771930245251724, -140.0293976192359935 ) ) ;
#19890 = CARTESIAN_POINT ( 'NONE',  ( -14.24457152944364680, -44.31067958253138528, -136.0552959530016892 ) ) ;
#19891 = VERTEX_POINT ( 'NONE', #5583 ) ;
#19892 = EDGE_CURVE ( 'NONE', #18676, #8637, #18325, .T. ) ;
#19893 = PLANE ( 'NONE',  #15907 ) ;
#19894 = EDGE_CURVE ( 'NONE', #1194, #963, #16531, .T. ) ;
#19895 = AXIS2_PLACEMENT_3D ( 'NONE', #9241, #12813, #14846 ) ;
#19896 = ORIENTED_EDGE ( 'NONE', *, *, #11989, .F. ) ;
#19897 = CARTESIAN_POINT ( 'NONE',  ( 1.759100530420000030, -16.38142836440000139, -142.5552959529999839 ) ) ;
#19898 = VERTEX_POINT ( 'NONE', #14741 ) ;
#19899 = CARTESIAN_POINT ( 'NONE',  ( 6.500000000000000000, 20.50000000000000000, -151.0552959529999839 ) ) ;
#19900 = CARTESIAN_POINT ( 'NONE',  ( -30.24848017571688175, 41.17617824351370359, -142.4709749654889208 ) ) ;
#19901 = MANIFOLD_SOLID_BREP ( 'lock_assembly.1\\Product1.1\\Part10.1\\PartBody', #8010 ) ;
#19902 = FACE_BOUND ( 'NONE', #13381, .T. ) ;
#19903 = CARTESIAN_POINT ( 'NONE',  ( 7.448738598091634522, 38.06998855381485924, -141.7958383015206891 ) ) ;
#19904 = ORIENTED_EDGE ( 'NONE', *, *, #11859, .F. ) ;
#19905 = FACE_OUTER_BOUND ( 'NONE', #23409, .T. ) ;
#19906 = CARTESIAN_POINT ( 'NONE',  ( -19.07674765109432613, 34.46746647540513209, -140.6674949932227889 ) ) ;
#19907 = CARTESIAN_POINT ( 'NONE',  ( -9.194386776583943544, 38.39074869067930251, -147.2010703919465300 ) ) ;
#19908 = DIRECTION ( 'NONE',  ( -0.7071067811865499042, 0.7071067811865451302, -1.776356839400251071E-12 ) ) ;
#19909 = ORIENTED_EDGE ( 'NONE', *, *, #15341, .T. ) ;
#19910 = CARTESIAN_POINT ( 'NONE',  ( 1.133692148650000009, 51.50000000000000000, -137.0552959530000123 ) ) ;
#19911 = SURFACE_STYLE_FILL_AREA ( #12640 ) ;
#19912 = ORIENTED_EDGE ( 'NONE', *, *, #984, .T. ) ;
#19913 = FACE_OUTER_BOUND ( 'NONE', #585, .T. ) ;
#19914 = CARTESIAN_POINT ( 'NONE',  ( -6.498948513140000216, 40.81543345029999870, -146.1568765789999986 ) ) ;
#19915 = DIRECTION ( 'NONE',  ( -0.1577507813030449846, -0.9874789572432817186, 8.298258002992369366E-13 ) ) ;
#19916 = ORIENTED_EDGE ( 'NONE', *, *, #18857, .F. ) ;
#19917 = EDGE_CURVE ( 'NONE', #9077, #8849, #12445, .T. ) ;
#19918 = CARTESIAN_POINT ( 'NONE',  ( -5.558768696205168780, 37.82651365787447872, -139.8085169319456043 ) ) ;
#19919 = CARTESIAN_POINT ( 'NONE',  ( 19.00000000000000000, 39.50000000000000000, -151.0552959529999839 ) ) ;
#19920 = EDGE_LOOP ( 'NONE', ( #21277, #1480, #13389, #1673 ) ) ;
#19921 = DIRECTION ( 'NONE',  ( 8.955190032050000935E-12, -9.104778821549999739E-13, 1.000000000000000000 ) ) ;
#19922 = CARTESIAN_POINT ( 'NONE',  ( -19.10036853998401085, 37.06903765908931803, -148.2030617969537616 ) ) ;
#19923 = DIRECTION ( 'NONE',  ( -2.257144641399999941E-12, 0.000000000000000000, -1.000000000000000000 ) ) ;
#19924 = CARTESIAN_POINT ( 'NONE',  ( -25.10891061336687358, 37.07005729393736004, -148.1636427047451718 ) ) ;
#19925 = PLANE ( 'NONE',  #2892 ) ;
#19926 = VECTOR ( 'NONE', #12758, 1000.000000000000000 ) ;
#19927 = CARTESIAN_POINT ( 'NONE',  ( -20.60824191589999899, -32.00000000000000000, -146.2257682199999920 ) ) ;
#19928 = FACE_OUTER_BOUND ( 'NONE', #1764, .T. ) ;
#19929 = CARTESIAN_POINT ( 'NONE',  ( 16.64676602990000021, -18.64223989710000140, -144.5552959529999839 ) ) ;
#19930 = DIRECTION ( 'NONE',  ( -1.000000000000000000, 0.000000000000000000, 2.257144641399999941E-12 ) ) ;
#19931 = ORIENTED_EDGE ( 'NONE', *, *, #6628, .F. ) ;
#19932 = ORIENTED_EDGE ( 'NONE', *, *, #12946, .T. ) ;
#19933 = FILL_AREA_STYLE ('',( #1981 ) ) ;
#19934 = B_SPLINE_CURVE_WITH_KNOTS ( 'NONE', 3,
 ( #22969, #2751, #12121, #964, #15356, #19271, #13441, #9979, #2981, #13917, #17013, #728, #7963, #20708, #4402, #11643, #18919, #9861 ),
 .UNSPECIFIED., .F., .F.,
 ( 4, 2, 2, 2, 2, 2, 2, 2, 4 ),
 ( 0.000000000000000000, 0.1250000000000000000, 0.2500000000000000000, 0.3750000000000000000, 0.5000000000000000000, 0.6250000000000000000, 0.7500000000000000000, 0.8750000000000000000, 1.000000000000000000 ),
 .UNSPECIFIED. ) ;
#19935 = ORIENTED_EDGE ( 'NONE', *, *, #7566, .T. ) ;
#19936 = CARTESIAN_POINT ( 'NONE',  ( -16.12052341118245380, 35.09110744045798924, -148.2635301759968343 ) ) ;
#19937 = DIRECTION ( 'NONE',  ( 2.257171095940000041E-12, 1.003664318210000046E-28, 1.000000000000000000 ) ) ;
#19938 = DIRECTION ( 'NONE',  ( 1.000000000000000000, 0.000000000000000000, -1.498801083243961330E-13 ) ) ;
#19939 = CARTESIAN_POINT ( 'NONE',  ( 14.00000000000000000, 20.50000000000000000, -136.0552959530000123 ) ) ;
#19940 = ORIENTED_EDGE ( 'NONE', *, *, #16320, .T. ) ;
#19941 = EDGE_CURVE ( 'NONE', #14581, #11240, #4620, .T. ) ;
#19942 = LINE ( 'NONE', #83, #6063 ) ;
#19943 = CARTESIAN_POINT ( 'NONE',  ( -20.45144833149999997, 36.94873838139999833, -139.8044047869999815 ) ) ;
#19944 = CARTESIAN_POINT ( 'NONE',  ( -11.97832217620000073, 39.59660284089999749, -147.8163995769999985 ) ) ;
#19945 = EDGE_CURVE ( 'NONE', #14843, #14816, #6277, .T. ) ;
#19946 = DIRECTION ( 'NONE',  ( 0.000000000000000000, 1.000000000000000000, 2.273736754430000208E-12 ) ) ;
#19947 = ORIENTED_EDGE ( 'NONE', *, *, #4952, .F. ) ;
#19948 = DIRECTION ( 'NONE',  ( 0.7071067811865473507, -0.7071067811865477948, -1.595945597898661113E-12 ) ) ;
#19949 = ORIENTED_EDGE ( 'NONE', *, *, #21562, .F. ) ;
#19950 = CARTESIAN_POINT ( 'NONE',  ( 8.749149998575488141, 35.52078178699984790, -142.0398975025203470 ) ) ;
#19951 = DIRECTION ( 'NONE',  ( 2.256683728769999802E-12, 0.000000000000000000, 1.000000000000000000 ) ) ;
#19952 = DIRECTION ( 'NONE',  ( 0.000000000000000000, -1.000000000000000000, 0.000000000000000000 ) ) ;
#19953 = ORIENTED_EDGE ( 'NONE', *, *, #10435, .F. ) ;
#19954 = CARTESIAN_POINT ( 'NONE',  ( 19.13369214859999801, -50.50000000000000000, -150.0552959529999839 ) ) ;
#19955 = EDGE_LOOP ( 'NONE', ( #22959, #15772, #15065, #22991 ) ) ;
#19956 = AXIS2_PLACEMENT_3D ( 'NONE', #15708, #17613, #22970 ) ;
#19957 = FACE_OUTER_BOUND ( 'NONE', #1066, .T. ) ;
#19958 = DIRECTION ( 'NONE',  ( -2.257252162960000001E-12, 0.000000000000000000, -1.000000000000000000 ) ) ;
#19959 = ORIENTED_EDGE ( 'NONE', *, *, #15505, .F. ) ;
#19960 = CARTESIAN_POINT ( 'NONE',  ( -27.04496201379999931, 40.71797592360000095, -143.5957174049999878 ) ) ;
#19961 = VERTEX_POINT ( 'NONE', #6632 ) ;
#19962 = CARTESIAN_POINT ( 'NONE',  ( -20.95225485081686045, 36.93199168239783603, -148.3394883767275019 ) ) ;
#19963 =( GEOMETRIC_REPRESENTATION_CONTEXT ( 3 ) GLOBAL_UNCERTAINTY_ASSIGNED_CONTEXT ( ( #8258 ) ) GLOBAL_UNIT_ASSIGNED_CONTEXT ( ( #2820, #8039, #9817 ) ) REPRESENTATION_CONTEXT ( 'NONE', 'WORKASPACE' ) );
#19964 = DIRECTION ( 'NONE',  ( -3.994014902950000436E-29, 1.000000000000000000, -4.148443855749999753E-27 ) ) ;
#19965 = ORIENTED_EDGE ( 'NONE', *, *, #8137, .F. ) ;
#19966 = SURFACE_STYLE_USAGE ( .BOTH. , #14259 ) ;
#19967 = VERTEX_POINT ( 'NONE', #15438 ) ;
#19968 = CARTESIAN_POINT ( 'NONE',  ( -26.45246943592391631, 41.22394968972064788, -141.5932472704602958 ) ) ;
#19969 = CARTESIAN_POINT ( 'NONE',  ( -10.43323856990612342, 37.07027821888498664, -139.9576636760149597 ) ) ;
#19970 = ORIENTED_EDGE ( 'NONE', *, *, #8959, .F. ) ;
#19971 = EDGE_CURVE ( 'NONE', #5099, #8186, #15687, .T. ) ;
#19972 = CARTESIAN_POINT ( 'NONE',  ( 8.890149109412865513, -17.38667989274045311, -145.5552959530314467 ) ) ;
#19973 = CARTESIAN_POINT ( 'NONE',  ( 19.13369214859999801, -51.50000000000000000, -150.0552959529999839 ) ) ;
#19974 = LINE ( 'NONE', #5101, #3757 ) ;
#19975 = ORIENTED_EDGE ( 'NONE', *, *, #3959, .T. ) ;
#19976 = DIRECTION ( 'NONE',  ( 0.9985681355238719137, -0.05349466063429310358, -4.512926597569420539E-12 ) ) ;
#19977 = AXIS2_PLACEMENT_3D ( 'NONE', #13013, #21843, #14458 ) ;
#19978 = AXIS2_PLACEMENT_3D ( 'NONE', #20892, #4582, #19098 ) ;
#19979 = CARTESIAN_POINT ( 'NONE',  ( -9.394779979509999990, -17.86685386420000299, -143.5552959529999839 ) ) ;
#19980 = ADVANCED_FACE ( 'NONE', ( #19374 ), #1057, .T. ) ;
#19981 = ORIENTED_EDGE ( 'NONE', *, *, #18978, .F. ) ;
#19982 = CARTESIAN_POINT ( 'NONE',  ( 5.276897646250000129, -21.39828525539999760, -145.5552959529999839 ) ) ;
#19983 = LINE ( 'NONE', #9137, #2484 ) ;
#19984 = CARTESIAN_POINT ( 'NONE',  ( -16.85333322537449519, 40.81111939231837482, -141.8642558381071694 ) ) ;
#19985 = CARTESIAN_POINT ( 'NONE',  ( -28.92883298428190031, 41.10844391202770254, -142.6522296194680166 ) ) ;
#19986 = ORIENTED_EDGE ( 'NONE', *, *, #4998, .F. ) ;
#19987 =( LENGTH_UNIT ( ) NAMED_UNIT ( * ) SI_UNIT ( .MILLI., .METRE. ) );
#19988 = LINE ( 'NONE', #10691, #13906 ) ;
#19989 =( BOUNDED_CURVE ( )  B_SPLINE_CURVE ( 5, ( #18929, #8325, #22864, #6432, #1331, #4533 ),
 .UNSPECIFIED., .F., .F. ) 
 B_SPLINE_CURVE_WITH_KNOTS ( ( 6, 6 ),
 ( 1.570796326852883729, 3.141592653590000062 ),
 .UNSPECIFIED. ) 
 CURVE ( )  GEOMETRIC_REPRESENTATION_ITEM ( )  RATIONAL_B_SPLINE_CURVE ( ( 0.2500000000000000000, 0.2500000000073699935, 0.3000000000110549792, 0.4000000000147399537, 0.6000000000147399648, 1.000000000000000000 ) ) 
 REPRESENTATION_ITEM ( '' )  );
#19990 = EDGE_CURVE ( 'NONE', #947, #13431, #17224, .T. ) ;
#19991 = DIRECTION ( 'NONE',  ( 1.000000000000000000, 3.994014904670000134E-29, -2.423380700840000070E-27 ) ) ;
#19992 = PLANE ( 'NONE',  #18233 ) ;
#19993 = DIRECTION ( 'NONE',  ( -1.211690350419999855E-27, -2.765629237170000203E-27, 1.000000000000000000 ) ) ;
#19994 = DIRECTION ( 'NONE',  ( 1.000000000000000000, 0.000000000000000000, -8.955799065309598247E-12 ) ) ;
#19995 = VECTOR ( 'NONE', #132, 1000.000000000000000 ) ;
#19996 = VECTOR ( 'NONE', #12743, 1000.000000000000000 ) ;
#19997 = ORIENTED_EDGE ( 'NONE', *, *, #3286, .T. ) ;
#19998 = SURFACE_SIDE_STYLE ('',( #21797 ) ) ;
#19999 = EDGE_CURVE ( 'NONE', #2935, #16387, #22949, .T. ) ;
#20000 = CARTESIAN_POINT ( 'NONE',  ( 25.50000000000000000, 25.50000000000000000, -136.0552959530000123 ) ) ;
#20001 = DIRECTION ( 'NONE',  ( -1.000000000000000000, 0.000000000000000000, 0.000000000000000000 ) ) ;
#20002 = B_SPLINE_CURVE_WITH_KNOTS ( 'NONE', 5,
 ( #9315, #18739, #423, #779, #5764, #18493, #14931, #22302, #14820, #5877, #651, #9667 ),
 .UNSPECIFIED., .F., .F.,
 ( 6, 3, 3, 6 ),
 ( 0.000000000000000000, 4.570086947620000117, 8.869210483019999813, 12.91901055009999943 ),
 .UNSPECIFIED. ) ;
#20003 = CARTESIAN_POINT ( 'NONE',  ( -5.958543189560369768, 38.89133234075744383, -148.3841615053280805 ) ) ;
#20004 = CARTESIAN_POINT ( 'NONE',  ( -32.50000000000000000, 76.00000000000000000, -155.5552959529999839 ) ) ;
#20005 = VERTEX_POINT ( 'NONE', #13415 ) ;
#20006 = CARTESIAN_POINT ( 'NONE',  ( -27.30725598840000146, 40.30964169850000189, -145.9048855949999961 ) ) ;
#20007 = DIRECTION ( 'NONE',  ( -0.06298685227120542907, -0.9980143568310855251, 1.515824502950130739E-13 ) ) ;
#20008 = VERTEX_POINT ( 'NONE', #17462 ) ;
#20009 = EDGE_CURVE ( 'NONE', #21283, #7036, #3079, .T. ) ;
#20010 = VECTOR ( 'NONE', #8955, 1000.000000000000000 ) ;
#20011 = ORIENTED_EDGE ( 'NONE', *, *, #6908, .T. ) ;
#20012 = EDGE_CURVE ( 'NONE', #22329, #11927, #21047, .T. ) ;
#20013 = CARTESIAN_POINT ( 'NONE',  ( -24.78261485200000180, 38.62237172060000034, -147.6366313890000015 ) ) ;
#20014 = B_SPLINE_CURVE_WITH_KNOTS ( 'NONE', 3,
 ( #23281, #6970, #14236, #21500, #19706, #10641, #4227, #2098, #11573, #16483, #11115, #9319, #18388, #16592, #3882, #22195, #1994, #7666 ),
 .UNSPECIFIED., .F., .F.,
 ( 4, 2, 2, 2, 2, 2, 2, 2, 4 ),
 ( 0.000000000000000000, 0.1250000000000000000, 0.2500000000000000000, 0.3750000000000000000, 0.5000000000000000000, 0.6250000000000000000, 0.7500000000000000000, 0.8750000000000000000, 1.000000000000000000 ),
 .UNSPECIFIED. ) ;
#20015 = DIRECTION ( 'NONE',  ( 0.000000000000000000, -1.000000000000000000, 0.000000000000000000 ) ) ;
#20016 = MANIFOLD_SOLID_BREP ( 'lock_assembly.1\\Product1.1\\PIN.1\\PartBody', #14115 ) ;
#20017 = CARTESIAN_POINT ( 'NONE',  ( 25.50000000000000000, 25.50000000000000000, -137.0552959530000123 ) ) ;
#20018 = CARTESIAN_POINT ( 'NONE',  ( 7.261465936361774176, 37.84621284174770039, -141.7028596377083147 ) ) ;
#20019 = ORIENTED_EDGE ( 'NONE', *, *, #11113, .F. ) ;
#20020 = SURFACE_SIDE_STYLE ('',( #8932 ) ) ;
#20021 = CARTESIAN_POINT ( 'NONE',  ( -19.36113520410000177, 33.15198947340000046, -146.5298456060000092 ) ) ;
#20022 = EDGE_CURVE ( 'NONE', #22145, #22886, #2728, .T. ) ;
#20023 = CARTESIAN_POINT ( 'NONE',  ( -9.072898850179999641, 36.94639249900000522, -148.2684494029999769 ) ) ;
#20024 = DIRECTION ( 'NONE',  ( 0.000000000000000000, 0.000000000000000000, 1.000000000000000000 ) ) ;
#20025 = CARTESIAN_POINT ( 'NONE',  ( 4.999999999879999990, -5.500000000000000000, -135.0552959530000123 ) ) ;
#20026 = ORIENTED_EDGE ( 'NONE', *, *, #7473, .T. ) ;
#20027 = EDGE_CURVE ( 'NONE', #2330, #22041, #5445, .T. ) ;
#20028 = DIRECTION ( 'NONE',  ( 0.6459422414661291079, 0.7633862853691523176, 2.273736754430455399E-12 ) ) ;
#20029 = EDGE_CURVE ( 'NONE', #2371, #7237, #11760, .T. ) ;
#20030 = VECTOR ( 'NONE', #18982, 1000.000000000000000 ) ;
#20031 = CYLINDRICAL_SURFACE ( 'NONE', #848, 1.499999999999996225 ) ;
#20032 = CARTESIAN_POINT ( 'NONE',  ( -5.558768696030000456, 37.82651365799999610, -139.8085169320000034 ) ) ;
#20033 = DIRECTION ( 'NONE',  ( 1.000000000000000000, 0.000000000000000000, -4.510281037539699253E-12 ) ) ;
#20034 = ORIENTED_EDGE ( 'NONE', *, *, #5158, .F. ) ;
#20035 = CARTESIAN_POINT ( 'NONE',  ( -6.346791270776173555, 40.13779649986400955, -145.7921771525873567 ) ) ;
#20036 = LINE ( 'NONE', #17771, #20518 ) ;
#20037 = ORIENTED_EDGE ( 'NONE', *, *, #8128, .F. ) ;
#20038 = FACE_OUTER_BOUND ( 'NONE', #9598, .T. ) ;
#20039 = PLANE ( 'NONE',  #5676 ) ;
#20040 = CARTESIAN_POINT ( 'NONE',  ( -34.50000000000000000, 26.00000000000000000, -139.5552959529999839 ) ) ;
#20041 = CARTESIAN_POINT ( 'NONE',  ( -24.06602356352919969, 36.94557182214808222, -148.2530914607175703 ) ) ;
#20042 = AXIS2_PLACEMENT_3D ( 'NONE', #3511, #16243, #10623 ) ;
#20043 = LINE ( 'NONE', #2084, #21531 ) ;
#20044 = B_SPLINE_CURVE_WITH_KNOTS ( 'NONE', 3,
 ( #733, #17371, #4527, #8088, #15359, #7970 ),
 .UNSPECIFIED., .F., .F.,
 ( 4, 2, 4 ),
 ( 0.000000000000000000, 0.5000000000000000000, 1.000000000000000000 ),
 .UNSPECIFIED. ) ;
#20045 = DIRECTION ( 'NONE',  ( 4.510774274160000731E-12, -1.321907670990000086E-13, 1.000000000000000000 ) ) ;
#20046 = SHAPE_DEFINITION_REPRESENTATION ( #1199, #15114 ) ;
#20047 = FACE_OUTER_BOUND ( 'NONE', #21802, .T. ) ;
#20048 = FACE_OUTER_BOUND ( 'NONE', #22579, .T. ) ;
#20049 = FACE_OUTER_BOUND ( 'NONE', #14184, .T. ) ;
#20050 = ORIENTED_EDGE ( 'NONE', *, *, #20568, .F. ) ;
#20051 = ADVANCED_FACE ( 'NONE', ( #23530 ), #3658, .F. ) ;
#20052 = ORIENTED_EDGE ( 'NONE', *, *, #15186, .T. ) ;
#20053 = ORIENTED_EDGE ( 'NONE', *, *, #17458, .F. ) ;
#20054 = CARTESIAN_POINT ( 'NONE',  ( -16.69741762601382717, 33.17454851232909618, -146.1538744914665244 ) ) ;
#20055 = CARTESIAN_POINT ( 'NONE',  ( 10.93320006080000084, -15.50000000000000000, -148.5552959529999839 ) ) ;
#20056 = CARTESIAN_POINT ( 'NONE',  ( 2.508811538200000246, -14.35090895149999923, -144.5552959529999839 ) ) ;
#20057 = CARTESIAN_POINT ( 'NONE',  ( 13.61765588496502843, 22.91567315748345024, -136.0552959530307362 ) ) ;
#20058 = AXIS2_PLACEMENT_3D ( 'NONE', #10094, #13558, #17370 ) ;
#20059 = EDGE_LOOP ( 'NONE', ( #19662, #22384, #11392, #3897 ) ) ;
#20060 = DIRECTION ( 'NONE',  ( 0.000000000000000000, 1.000000000000000000, 0.000000000000000000 ) ) ;
#20061 = CARTESIAN_POINT ( 'NONE',  ( -19.36113520410000177, 33.15198947340000046, -146.5298456060000092 ) ) ;
#20062 = VECTOR ( 'NONE', #8200, 1000.000000000000000 ) ;
#20063 = CARTESIAN_POINT ( 'NONE',  ( 13.13369214859999978, -51.50000000000000000, -137.0552959530000123 ) ) ;
#20064 = ORIENTED_EDGE ( 'NONE', *, *, #554, .F. ) ;
#20065 = DIRECTION ( 'NONE',  ( -0.9954742291034677226, 0.09503188512734457583, 4.502513436702118395E-12 ) ) ;
#20066 = ORIENTED_EDGE ( 'NONE', *, *, #22649, .T. ) ;
#20067 = CARTESIAN_POINT ( 'NONE',  ( 9.543956954615813615, 35.92288351715210126, -141.7992203786431276 ) ) ;
#20068 = LINE ( 'NONE', #9443, #18077 ) ;
#20069 = PLANE ( 'NONE',  #11264 ) ;
#20070 = ORIENTED_EDGE ( 'NONE', *, *, #18715, .F. ) ;
#20071 = ADVANCED_FACE ( 'NONE', ( #19957 ), #12330, .T. ) ;
#20072 = AXIS2_PLACEMENT_3D ( 'NONE', #1953, #15008, #5959 ) ;
#20073 = ADVANCED_FACE ( 'NONE', ( #1537 ), #7228, .T. ) ;
#20074 = DIRECTION ( 'NONE',  ( 0.000000000000000000, 0.000000000000000000, -1.000000000000000000 ) ) ;
#20075 = EDGE_LOOP ( 'NONE', ( #18047, #8694, #15294, #23367 ) ) ;
#20076 = DIRECTION ( 'NONE',  ( -2.688820921349999492E-17, 1.000000000000000000, 6.069065783950000909E-29 ) ) ;
#20077 = ADVANCED_FACE ( 'NONE', ( #6988 ), #10773, .T. ) ;
#20078 = LINE ( 'NONE', #19727, #15039 ) ;
#20079 = EDGE_LOOP ( 'NONE', ( #21978, #16992, #21180, #5922 ) ) ;
#20080 = CARTESIAN_POINT ( 'NONE',  ( -25.89998524117842393, 37.72641173383139801, -140.6959480270122640 ) ) ;
#20081 = ORIENTED_EDGE ( 'NONE', *, *, #14777, .T. ) ;
#20082 = CARTESIAN_POINT ( 'NONE',  ( -23.22224815339999893, 34.57381638260000045, -140.7548632179999970 ) ) ;
#20083 = CARTESIAN_POINT ( 'NONE',  ( -5.499999999959999997, 44.50000000000000000, -136.0552959530000123 ) ) ;
#20084 = EDGE_LOOP ( 'NONE', ( #11476, #8897, #2093, #10572 ) ) ;
#20085 = DIRECTION ( 'NONE',  ( 1.000000000000000000, 0.000000000000000000, 0.000000000000000000 ) ) ;
#20086 = VERTEX_POINT ( 'NONE', #23410 ) ;
#20087 = LINE ( 'NONE', #7354, #4551 ) ;
#20088 = CARTESIAN_POINT ( 'NONE',  ( -24.97797643630000053, 37.05442817780000553, -147.8575004449999994 ) ) ;
#20089 = CARTESIAN_POINT ( 'NONE',  ( -9.766576661180000229, -18.00000000000000000, -145.5657682190000060 ) ) ;
#20090 = PLANE ( 'NONE',  #9798 ) ;
#20091 = CARTESIAN_POINT ( 'NONE',  ( -32.00000000000000000, -50.00000000000000000, -149.5552959529999839 ) ) ;
#20092 = EDGE_CURVE ( 'NONE', #10473, #18841, #16274, .T. ) ;
#20093 = VECTOR ( 'NONE', #5652, 1000.000000000000000 ) ;
#20094 = CARTESIAN_POINT ( 'NONE',  ( -9.434278515689999978, -18.41834002140000237, -147.5552959529999839 ) ) ;
#20095 = ORIENTED_EDGE ( 'NONE', *, *, #22316, .T. ) ;
#20096 = AXIS2_PLACEMENT_3D ( 'NONE', #8555, #6552, #13820 ) ;
#20097 = CARTESIAN_POINT ( 'NONE',  ( 32.14594224149999491, 40.79958733410000349, -142.8052959529999839 ) ) ;
#20098 = CARTESIAN_POINT ( 'NONE',  ( 8.697346895277828338, 35.50958615751394376, -146.0625927866750260 ) ) ;
#20099 = VECTOR ( 'NONE', #3562, 1000.000000000000000 ) ;
#20100 = ORIENTED_EDGE ( 'NONE', *, *, #20435, .F. ) ;
#20101 = CARTESIAN_POINT ( 'NONE',  ( 3.580113616945115318, -4.700859805997813723, -150.0552959529999839 ) ) ;
#20102 = DIRECTION ( 'NONE',  ( -8.954614827420000395E-12, 9.094947017729999296E-13, -1.000000000000000000 ) ) ;
#20103 = EDGE_CURVE ( 'NONE', #404, #2894, #17590, .T. ) ;
#20104 = FACE_BOUND ( 'NONE', #8670, .T. ) ;
#20105 = CARTESIAN_POINT ( 'NONE',  ( -3.500000000000000000, 46.50000000000000000, -150.5552959529999839 ) ) ;
#20106 = VERTEX_POINT ( 'NONE', #3423 ) ;
#20107 = DIRECTION ( 'NONE',  ( 0.000000000000000000, 0.000000000000000000, -1.000000000000000000 ) ) ;
#20108 = EDGE_CURVE ( 'NONE', #6084, #8391, #1302, .T. ) ;
#20109 = DIRECTION ( 'NONE',  ( -1.701177084980000217E-20, 2.602084704489999637E-17, -1.000000000000000000 ) ) ;
#20110 = AXIS2_PLACEMENT_3D ( 'NONE', #10495, #7307, #16354 ) ;
#20111 = CARTESIAN_POINT ( 'NONE',  ( 7.750000000030000002, -39.98606797749999942, -137.0552959530000123 ) ) ;
#20112 = DIRECTION ( 'NONE',  ( 0.000000000000000000, 1.000000000000000000, 0.000000000000000000 ) ) ;
#20113 = CARTESIAN_POINT ( 'NONE',  ( -17.97686571119999854, 41.53571570570000659, -143.4577736070000071 ) ) ;
#20114 = DIRECTION ( 'NONE',  ( 0.000000000000000000, -1.000000000000000000, 0.000000000000000000 ) ) ;
#20115 = CIRCLE ( 'NONE', #2633, 15.00000000000000000 ) ;
#20116 = ORIENTED_EDGE ( 'NONE', *, *, #21618, .F. ) ;
#20117 = CARTESIAN_POINT ( 'NONE',  ( -15.31679993919999916, -18.00000000000000000, -148.5552959529999839 ) ) ;
#20118 = VECTOR ( 'NONE', #19823, 1000.000000000000000 ) ;
#20119 = PRODUCT_DEFINITION ( 'UNKNOWN', '', #8864, #8732 ) ;
#20120 = CARTESIAN_POINT ( 'NONE',  ( -4.192924954330000453, -28.60725908990000121, -146.0552959529999839 ) ) ;
#20121 = AXIS2_PLACEMENT_3D ( 'NONE', #3918, #12710, #18660 ) ;
#20122 = DIRECTION ( 'NONE',  ( -3.994014902950000436E-29, 1.000000000000000000, -4.148443855749999753E-27 ) ) ;
#20123 = CARTESIAN_POINT ( 'NONE',  ( -5.832642628619999492, 38.59814668869999821, -147.7665506369999662 ) ) ;
#20124 = LINE ( 'NONE', #8805, #14235 ) ;
#20125 = ORIENTED_EDGE ( 'NONE', *, *, #22728, .F. ) ;
#20126 = PLANE ( 'NONE',  #8673 ) ;
#20127 = PLANE ( 'NONE',  #21993 ) ;
#20128 = VERTEX_POINT ( 'NONE', #17700 ) ;
#20129 = AXIS2_PLACEMENT_3D ( 'NONE', #17219, #2719, #19125 ) ;
#20130 = EDGE_CURVE ( 'NONE', #19030, #19493, #14755, .T. ) ;
#20131 =( REPRESENTATION_RELATIONSHIP ('NONE','NONE', #7672, #23186 ) REPRESENTATION_RELATIONSHIP_WITH_TRANSFORMATION ( #10744 )SHAPE_REPRESENTATION_RELATIONSHIP( ) );
#20132 = VECTOR ( 'NONE', #15821, 1000.000000000000000 ) ;
#20133 = ORIENTED_EDGE ( 'NONE', *, *, #13531, .F. ) ;
#20134 = VECTOR ( 'NONE', #7917, 1000.000000000000000 ) ;
#20135 =( BOUNDED_CURVE ( )  B_SPLINE_CURVE ( 5, ( #12261, #21325, #14057, #18417, #12936, #12143, #23336, #19417, #7460, #12492, #8676, #17865 ),
 .UNSPECIFIED., .F., .F. ) 
 B_SPLINE_CURVE_WITH_KNOTS ( ( 6, 3, 3, 6 ),
 ( 0.000000000000000000, 4.346865784160000246, 8.778337911509998648, 13.29702284770000098 ),
 .UNSPECIFIED. ) 
 CURVE ( )  GEOMETRIC_REPRESENTATION_ITEM ( )  RATIONAL_B_SPLINE_CURVE ( ( 0.2500000000000000000, 0.2500000000000000000, 0.2500000000000000000, 0.2500000000000000000, 0.2500000000000000000, 0.2500000000000000000, 0.2500000000000000000, 0.2500000000000000000, 0.2500000000000000000, 0.2500000000000000000, 0.2500000000000000000, 0.2500000000000000000 ) ) 
 REPRESENTATION_ITEM ( '' )  );
#20136 = AXIS2_PLACEMENT_3D ( 'NONE', #20553, #19226, #1287 ) ;
#20137 = CARTESIAN_POINT ( 'NONE',  ( 6.000000000010000001, -3.500000000000000000, -136.0552959530000123 ) ) ;
#20138 = DIRECTION ( 'NONE',  ( 1.000000000000000000, 0.000000000000000000, -8.955534726494208689E-12 ) ) ;
#20139 = VECTOR ( 'NONE', #8841, 1000.000000000000000 ) ;
#20140 = VECTOR ( 'NONE', #13910, 1000.000000000000000 ) ;
#20141 = DIRECTION ( 'NONE',  ( 0.000000000000000000, 1.000000000000000000, 0.000000000000000000 ) ) ;
#20142 = CARTESIAN_POINT ( 'NONE',  ( -21.35824191589999899, -4.000000000000000000, -150.0657682190000060 ) ) ;
#20143 = ORIENTED_EDGE ( 'NONE', *, *, #2440, .T. ) ;
#20144 = FILL_AREA_STYLE_COLOUR ( '', #19269 ) ;
#20145 = EDGE_CURVE ( 'NONE', #10397, #4660, #4480, .T. ) ;
#20146 = CARTESIAN_POINT ( 'NONE',  ( -18.75678166064549757, 32.44474377655248531, -143.7296912422551429 ) ) ;
#20147 = DIRECTION ( 'NONE',  ( 0.000000000000000000, 1.000000000000000000, 0.000000000000000000 ) ) ;
#20148 = PLANE ( 'NONE',  #23253 ) ;
#20149 = DIRECTION ( 'NONE',  ( -0.7071067811865474617, 0.7071067811865476838, 0.000000000000000000 ) ) ;
#20150 = CARTESIAN_POINT ( 'NONE',  ( 18.09808825521564657, 20.66051412330947556, -136.0552959530408259 ) ) ;
#20151 = ADVANCED_FACE ( 'NONE', ( #8635 ), #15910, .T. ) ;
#20152 = DIRECTION ( 'NONE',  ( 0.6459422414661299960, 0.7633862853691516515, 2.257453483404490485E-12 ) ) ;
#20153 = CARTESIAN_POINT ( 'NONE',  ( -4.946601369560000627, -23.77962690289999870, -143.5552959529999839 ) ) ;
#20154 = CARTESIAN_POINT ( 'NONE',  ( -6.719053507368635714, 25.42349012523353480, -136.0552959529848636 ) ) ;
#20155 = VECTOR ( 'NONE', #12526, 1000.000000000000227 ) ;
#20156 = AXIS2_PLACEMENT_3D ( 'NONE', #8242, #4694, #22778 ) ;
#20157 = ORIENTED_EDGE ( 'NONE', *, *, #3854, .F. ) ;
#20158 = VECTOR ( 'NONE', #4819, 1000.000000000000000 ) ;
#20159 = CARTESIAN_POINT ( 'NONE',  ( -6.033650297970000409, 36.94170754819999303, -147.9652040070000112 ) ) ;
#20160 = ORIENTED_EDGE ( 'NONE', *, *, #16627, .T. ) ;
#20161 = CARTESIAN_POINT ( 'NONE',  ( 19.13369214859999801, 51.00000000000000000, -149.5552959529999839 ) ) ;
#20162 = EDGE_CURVE ( 'NONE', #9674, #3481, #20201, .T. ) ;
#20163 = PLANE ( 'NONE',  #13655 ) ;
#20164 = EDGE_CURVE ( 'NONE', #20657, #16830, #16437, .T. ) ;
#20165 = CARTESIAN_POINT ( 'NONE',  ( 23.21181482501885185, -23.48612613683581785, -148.5552959530001260 ) ) ;
#20166 = CARTESIAN_POINT ( 'NONE',  ( -17.08912089869999917, -34.50000000000000000, -147.1421200419999877 ) ) ;
#20167 = CARTESIAN_POINT ( 'NONE',  ( -13.04270098972981984, 34.92521805811855984, -147.0831430691404194 ) ) ;
#20168 = EDGE_CURVE ( 'NONE', #21310, #18719, #14837, .T. ) ;
#20169 = FACE_OUTER_BOUND ( 'NONE', #21190, .T. ) ;
#20170 = EDGE_CURVE ( 'NONE', #14107, #10473, #13268, .T. ) ;
#20171 = LINE ( 'NONE', #15624, #11638 ) ;
#20172 = CARTESIAN_POINT ( 'NONE',  ( -32.50000000000000000, -36.00000000000000000, -151.0552959529999839 ) ) ;
#20173 = VECTOR ( 'NONE', #12367, 1000.000000000000000 ) ;
#20174 = CYLINDRICAL_SURFACE ( 'NONE', #1733, 0.5000000000000079936 ) ;
#20175 = AXIS2_PLACEMENT_3D ( 'NONE', #16025, #23286, #6978 ) ;
#20176 = LINE ( 'NONE', #12895, #3338 ) ;
#20177 = ORIENTED_EDGE ( 'NONE', *, *, #13614, .F. ) ;
#20178 = UNCERTAINTY_MEASURE_WITH_UNIT (LENGTH_MEASURE( 1.000000000000000082E-05 ), #15158, 'distance_accuracy_value', 'NONE');
#20179 = EDGE_LOOP ( 'NONE', ( #13848, #1913, #19479, #17054, #2173 ) ) ;
#20180 = FILL_AREA_STYLE_COLOUR ( '', #483 ) ;
#20181 = MANIFOLD_SOLID_BREP ( 'lock_assembly.1\\Part1.3\\PartBody', #11059 ) ;
#20182 = ORIENTED_EDGE ( 'NONE', *, *, #12431, .F. ) ;
#20183 = CARTESIAN_POINT ( 'NONE',  ( -12.94305406498005162, 37.05025962682652363, -148.5780888799759794 ) ) ;
#20184 = DIRECTION ( 'NONE',  ( 1.526468026909999897E-13, 8.159623473500000156E-13, 1.000000000000000000 ) ) ;
#20185 = CARTESIAN_POINT ( 'NONE',  ( 25.31684607429999900, 45.26810052439999765, -136.0552959530000123 ) ) ;
#20186 = ORIENTED_EDGE ( 'NONE', *, *, #12393, .T. ) ;
#20187 = PLANE ( 'NONE',  #19004 ) ;
#20188 = CARTESIAN_POINT ( 'NONE',  ( -19.89396978539216576, 32.81765722514309402, -143.8793666190109661 ) ) ;
#20189 = CARTESIAN_POINT ( 'NONE',  ( 4.500000000000000000, -3.500000000000000000, -145.5552959529999839 ) ) ;
#20190 = AXIS2_PLACEMENT_3D ( 'NONE', #11616, #1054, #829 ) ;
#20191 = VERTEX_POINT ( 'NONE', #1888 ) ;
#20192 = VECTOR ( 'NONE', #17280, 1000.000000000000000 ) ;
#20193 = CARTESIAN_POINT ( 'NONE',  ( -20.82021697191324705, 38.61793539557643129, -140.2922895080757257 ) ) ;
#20194 = CARTESIAN_POINT ( 'NONE',  ( 9.901116376611746261, 37.53576186991580954, -141.6133621760922665 ) ) ;
#20195 = EDGE_CURVE ( 'NONE', #8763, #7782, #18637, .T. ) ;
#20196 = CARTESIAN_POINT ( 'NONE',  ( 8.931951867280000457, -17.52729875919999714, -142.5552959529999839 ) ) ;
#20197 = CARTESIAN_POINT ( 'NONE',  ( 1.500000000000000000, -3.500000000000000000, -150.0552959529999839 ) ) ;
#20198 = EDGE_LOOP ( 'NONE', ( #6602, #7947, #489, #21753 ) ) ;
#20199 = DIRECTION ( 'NONE',  ( 0.000000000000000000, 0.000000000000000000, 1.000000000000000000 ) ) ;
#20200 = ORIENTED_EDGE ( 'NONE', *, *, #1490, .F. ) ;
#20201 = LINE ( 'NONE', #18173, #16654 ) ;
#20202 = VECTOR ( 'NONE', #15088, 1000.000000000000000 ) ;
#20203 = AXIS2_PLACEMENT_3D ( 'NONE', #20117, #487, #3933 ) ;
#20204 = ORIENTED_EDGE ( 'NONE', *, *, #13438, .F. ) ;
#20205 = DIRECTION ( 'NONE',  ( 0.000000000000000000, 0.000000000000000000, 1.000000000000000000 ) ) ;
#20206 = VERTEX_POINT ( 'NONE', #9334 ) ;
#20207 = CARTESIAN_POINT ( 'NONE',  ( -23.41786221899999987, 36.12684018730000446, -140.1150171360000058 ) ) ;
#20208 = ORIENTED_EDGE ( 'NONE', *, *, #12652, .F. ) ;
#20209 = CARTESIAN_POINT ( 'NONE',  ( -29.64895016830000429, 40.48034887659999725, -142.7934167989999992 ) ) ;
#20210 = ORIENTED_EDGE ( 'NONE', *, *, #3052, .T. ) ;
#20211 = APPLICATION_PROTOCOL_DEFINITION ( 'draft international standard', 'automotive_design', 1998, #13127 ) ;
#20212 = ORIENTED_EDGE ( 'NONE', *, *, #3210, .F. ) ;
#20213 = LINE ( 'NONE', #14959, #18230 ) ;
#20214 = CARTESIAN_POINT ( 'NONE',  ( -23.61758233950000019, 37.78045452579999619, -140.0909254550000185 ) ) ;
#20215 = CARTESIAN_POINT ( 'NONE',  ( -23.18315392570000100, 51.50000000000000000, -137.0552959530000123 ) ) ;
#20216 = DIRECTION ( 'NONE',  ( 0.000000000000000000, -1.000000000000000000, 0.000000000000000000 ) ) ;
#20217 = CARTESIAN_POINT ( 'NONE',  ( -11.19828263951698055, 35.50589712222299710, -140.5907466442008058 ) ) ;
#20218 = ADVANCED_FACE ( 'NONE', ( #7792 ), #11236, .F. ) ;
#20219 = DIRECTION ( 'NONE',  ( 0.000000000000000000, 1.000000000000000000, 0.000000000000000000 ) ) ;
#20220 = ORIENTED_EDGE ( 'NONE', *, *, #6764, .F. ) ;
#20221 = DIRECTION ( 'NONE',  ( 1.000000000000000000, 0.000000000000000000, 0.000000000000000000 ) ) ;
#20222 = AXIS2_PLACEMENT_3D ( 'NONE', #20236, #22357, #14746 ) ;
#20223 = AXIS2_PLACEMENT_3D ( 'NONE', #15259, #15607, #7979 ) ;
#20224 = AXIS2_PLACEMENT_3D ( 'NONE', #18467, #13344, #11433 ) ;
#20225 = PLANE ( 'NONE',  #11353 ) ;
#20226 = ORIENTED_EDGE ( 'NONE', *, *, #21618, .T. ) ;
#20227 = CARTESIAN_POINT ( 'NONE',  ( -22.10824191589999899, -4.000000000000000000, -146.2257682199999920 ) ) ;
#20228 = CARTESIAN_POINT ( 'NONE',  ( -12.88538148427827679, 39.54446768249285071, -147.5580768661236277 ) ) ;
#20229 = CARTESIAN_POINT ( 'NONE',  ( -17.17121306734199493, 41.35383210599469095, -144.5122939762497936 ) ) ;
#20230 = CARTESIAN_POINT ( 'NONE',  ( -30.02200000005139913, 40.89711431701928035, -146.3052959529881889 ) ) ;
#20231 = ORIENTED_EDGE ( 'NONE', *, *, #6041, .T. ) ;
#20232 = FILL_AREA_STYLE ('',( #12955 ) ) ;
#20233 = CARTESIAN_POINT ( 'NONE',  ( -25.46206384041683535, 37.06683745569177546, -140.4480127388158905 ) ) ;
#20234 = ORIENTED_EDGE ( 'NONE', *, *, #1289, .F. ) ;
#20235 = CARTESIAN_POINT ( 'NONE',  ( -32.50000000000000000, 37.00000000000000000, -137.5552959530000123 ) ) ;
#20236 = CARTESIAN_POINT ( 'NONE',  ( 10.93320006080000084, -15.50000000000000000, -150.0552959529999839 ) ) ;
#20237 = DIRECTION ( 'NONE',  ( 0.000000000000000000, -1.000000000000000000, 0.000000000000000000 ) ) ;
#20238 = CARTESIAN_POINT ( 'NONE',  ( -19.64847913693946069, 38.01206741062298988, -139.5740658646235488 ) ) ;
#20239 = VERTEX_POINT ( 'NONE', #11019 ) ;
#20240 = VECTOR ( 'NONE', #11543, 1000.000000000000000 ) ;
#20241 = AXIS2_PLACEMENT_3D ( 'NONE', #21883, #10905, #3315 ) ;
#20242 = CARTESIAN_POINT ( 'NONE',  ( -27.16804840547268540, 34.58594410721605783, -147.1822449632341829 ) ) ;
#20243 = CARTESIAN_POINT ( 'NONE',  ( -31.00000000000000000, -36.00000000000000000, -151.0552959529999839 ) ) ;
#20244 = CARTESIAN_POINT ( 'NONE',  ( -12.47706116150000000, 35.17890886639999337, -148.2557368829999973 ) ) ;
#20245 = CARTESIAN_POINT ( 'NONE',  ( -12.50000000000000000, 25.50000000000000000, -151.0552959529999839 ) ) ;
#20246 = CARTESIAN_POINT ( 'NONE',  ( -3.499999999959999997, 44.50000000000000000, -136.0552959530000123 ) ) ;
#20247 = ORIENTED_EDGE ( 'NONE', *, *, #22379, .T. ) ;
#20248 = EDGE_CURVE ( 'NONE', #6873, #20386, #18296, .T. ) ;
#20249 = DIRECTION ( 'NONE',  ( -5.094701932209999624E-24, -1.000000000000000000, 1.149947916579999802E-35 ) ) ;
#20250 = CARTESIAN_POINT ( 'NONE',  ( 3.000000000000000000, -3.500000000000000000, -150.0552959529999839 ) ) ;
#20251 = EDGE_CURVE ( 'NONE', #8391, #10751, #16497, .T. ) ;
#20252 = ORIENTED_EDGE ( 'NONE', *, *, #1211, .F. ) ;
#20253 =( GEOMETRIC_REPRESENTATION_CONTEXT ( 3 ) GLOBAL_UNCERTAINTY_ASSIGNED_CONTEXT ( ( #21607 ) ) GLOBAL_UNIT_ASSIGNED_CONTEXT ( ( #3633, #9206, #18614 ) ) REPRESENTATION_CONTEXT ( 'NONE', 'WORKASPACE' ) );
#20254 = EDGE_LOOP ( 'NONE', ( #18627, #11214, #15223, #7752 ) ) ;
#20255 = CIRCLE ( 'NONE', #17195, 6.000000000000001776 ) ;
#20256 = CARTESIAN_POINT ( 'NONE',  ( -22.69591931514189298, 36.33656945782036729, -140.6974727659104758 ) ) ;
#20257 = CARTESIAN_POINT ( 'NONE',  ( -29.68301555213733423, 36.92109708053600770, -140.1550845752329053 ) ) ;
#20258 = DIRECTION ( 'NONE',  ( 5.968558980390000333E-14, -1.000000000000000000, 0.000000000000000000 ) ) ;
#20259 = LINE ( 'NONE', #11183, #13661 ) ;
#20260 = ORIENTED_EDGE ( 'NONE', *, *, #18652, .F. ) ;
#20261 = CARTESIAN_POINT ( 'NONE',  ( 4.750000000030000002, -35.98606797749999942, -136.5552959530000123 ) ) ;
#20262 = CARTESIAN_POINT ( 'NONE',  ( -18.91006587267516181, 33.19603641716903297, -143.7906546518633775 ) ) ;
#20263 = CYLINDRICAL_SURFACE ( 'NONE', #17400, 1.000000000000001332 ) ;
#20264 = DIRECTION ( 'NONE',  ( -2.602084704489999637E-17, 1.000000000000000000, 4.426606872070000353E-37 ) ) ;
#20265 = CARTESIAN_POINT ( 'NONE',  ( -23.47736846006178979, 41.31403509295417820, -141.6371185060827429 ) ) ;
#20266 = CARTESIAN_POINT ( 'NONE',  ( 10.55069612126581724, -19.50000000000000355, -148.5552959529999839 ) ) ;
#20267 = CARTESIAN_POINT ( 'NONE',  ( 7.500000000000000000, -3.500000000000000000, -150.0552959529999839 ) ) ;
#20268 = DIRECTION ( 'NONE',  ( 1.526468026909999897E-13, 8.159623473500000156E-13, 1.000000000000000000 ) ) ;
#20269 = STYLED_ITEM ( 'NONE', ( #1067 ), #22005 ) ;
#20270 = FACE_OUTER_BOUND ( 'NONE', #15236, .T. ) ;
#20271 = EDGE_LOOP ( 'NONE', ( #18850, #11731, #10433, #2132 ) ) ;
#20272 = CARTESIAN_POINT ( 'NONE',  ( -5.621737161624158041, 40.23839945177277855, -145.9417178035539848 ) ) ;
#20273 = EDGE_CURVE ( 'NONE', #7104, #3870, #18403, .T. ) ;
#20274 = EDGE_LOOP ( 'NONE', ( #13511, #21660, #9342, #18988 ) ) ;
#20275 = CARTESIAN_POINT ( 'NONE',  ( -14.47770030809999930, -34.50000000000000000, -147.5552959529999839 ) ) ;
#20276 = DIRECTION ( 'NONE',  ( -1.000000000000000000, 0.000000000000000000, 2.262368070660000099E-12 ) ) ;
#20277 = CARTESIAN_POINT ( 'NONE',  ( -24.73161923030975373, 36.03940581491394823, -148.7361830015362045 ) ) ;
#20278 = ORIENTED_EDGE ( 'NONE', *, *, #15963, .F. ) ;
#20279 = CARTESIAN_POINT ( 'NONE',  ( -13.02237250279999969, 32.42872598539999274, -144.6889042450000034 ) ) ;
#20280 = LINE ( 'NONE', #7649, #16206 ) ;
#20281 = ADVANCED_FACE ( 'NONE', ( #17433 ), #22441, .T. ) ;
#20282 = DIRECTION ( 'NONE',  ( 0.000000000000000000, 0.000000000000000000, 1.000000000000000000 ) ) ;
#20283 = DIRECTION ( 'NONE',  ( 0.000000000000000000, -1.000000000000000000, 2.257144641399999941E-12 ) ) ;
#20284 = DIRECTION ( 'NONE',  ( 0.000000000000000000, 0.000000000000000000, -1.000000000000000000 ) ) ;
#20285 = FACE_OUTER_BOUND ( 'NONE', #22332, .T. ) ;
#20286 = VECTOR ( 'NONE', #3755, 1000.000000000000000 ) ;
#20287 = ORIENTED_EDGE ( 'NONE', *, *, #20662, .F. ) ;
#20288 = DIRECTION ( 'NONE',  ( -0.7071067811865499042, -0.7071067811865451302, -1.776356839400251071E-12 ) ) ;
#20289 = ORIENTED_EDGE ( 'NONE', *, *, #10678, .F. ) ;
#20290 = SURFACE_SIDE_STYLE ('',( #5530 ) ) ;
#20291 = ADVANCED_FACE ( 'NONE', ( #4588 ), #8280, .T. ) ;
#20292 = EDGE_CURVE ( 'NONE', #11665, #10060, #18755, .T. ) ;
#20293 = EDGE_LOOP ( 'NONE', ( #22958, #10076, #20095, #22920 ) ) ;
#20294 = DIRECTION ( 'NONE',  ( 0.7633862853691524286, 0.6459422414661293299, 0.000000000000000000 ) ) ;
#20295 = DIRECTION ( 'NONE',  ( 0.000000000000000000, 1.000000000000000000, 0.000000000000000000 ) ) ;
#20296 = PLANE ( 'NONE',  #17231 ) ;
#20297 = EDGE_CURVE ( 'NONE', #9607, #2844, #13866, .T. ) ;
#20298 = ORIENTED_EDGE ( 'NONE', *, *, #3948, .F. ) ;
#20299 = CARTESIAN_POINT ( 'NONE',  ( 10.50000000020000002, 24.50000000000000000, -136.5552959530000123 ) ) ;
#20300 = EDGE_CURVE ( 'NONE', #15915, #16877, #15658, .T. ) ;
#20301 = CARTESIAN_POINT ( 'NONE',  ( -32.50000000000000000, 47.50000000000000000, -150.5552959529999839 ) ) ;
#20302 = CARTESIAN_POINT ( 'NONE',  ( -44.50000000000000000, 45.00000000000000000, -148.4460207619999892 ) ) ;
#20303 = ORIENTED_EDGE ( 'NONE', *, *, #11064, .T. ) ;
#20304 = CARTESIAN_POINT ( 'NONE',  ( -20.90175983535185011, 40.40386100034367445, -144.4637348342631356 ) ) ;
#20305 = VECTOR ( 'NONE', #9643, 1000.000000000000000 ) ;
#20306 = CARTESIAN_POINT ( 'NONE',  ( -17.18002735250068369, 36.98113687426175034, -140.6755148967653497 ) ) ;
#20307 = CARTESIAN_POINT ( 'NONE',  ( -0.9999999999639999082, 20.50000000000000000, -136.0552959530000123 ) ) ;
#20308 = CARTESIAN_POINT ( 'NONE',  ( -22.10824191589999899, -1.500000000000000000, -144.8157682190000060 ) ) ;
#20309 = ORIENTED_EDGE ( 'NONE', *, *, #16233, .T. ) ;
#20310 = DIRECTION ( 'NONE',  ( -1.000000000000000000, 0.000000000000000000, 0.000000000000000000 ) ) ;
#20311 = ORIENTED_EDGE ( 'NONE', *, *, #6723, .T. ) ;
#20312 = CARTESIAN_POINT ( 'NONE',  ( 19.84954298759999958, 51.20423285660000090, -150.0552959529999839 ) ) ;
#20313 = EDGE_LOOP ( 'NONE', ( #401, #12266, #18223, #1598, #1876 ) ) ;
#20314 = CARTESIAN_POINT ( 'NONE',  ( -27.30725598840000146, 40.30964169850000189, -145.9048855949999961 ) ) ;
#20315 = EDGE_CURVE ( 'NONE', #13630, #7372, #17197, .T. ) ;
#20316 = ORIENTED_EDGE ( 'NONE', *, *, #4229, .T. ) ;
#20317 = VECTOR ( 'NONE', #8215, 1000.000000000000000 ) ;
#20318 = CARTESIAN_POINT ( 'NONE',  ( -21.70515251718890326, 32.50310406744011971, -144.3999433124957363 ) ) ;
#20319 = ADVANCED_FACE ( 'NONE', ( #15531 ), #6365, .F. ) ;
#20320 = EDGE_LOOP ( 'NONE', ( #17734, #44, #15381, #1618 ) ) ;
#20321 = DIRECTION ( 'NONE',  ( 2.257144641399999941E-12, 0.000000000000000000, 1.000000000000000000 ) ) ;
#20322 = ORIENTED_EDGE ( 'NONE', *, *, #7416, .F. ) ;
#20323 = SHAPE_DEFINITION_REPRESENTATION ( #8812, #16641 ) ;
#20324 = EDGE_CURVE ( 'NONE', #3534, #7769, #4240, .T. ) ;
#20325 = ORIENTED_EDGE ( 'NONE', *, *, #13612, .F. ) ;
#20326 = CARTESIAN_POINT ( 'NONE',  ( -29.45815224828859868, 36.94793816027001299, -140.4653836173399952 ) ) ;
#20327 = CARTESIAN_POINT ( 'NONE',  ( -14.74965217829999986, 40.59671102100000439, -143.6490422509999973 ) ) ;
#20328 = CARTESIAN_POINT ( 'NONE',  ( -6.683153925719999222, -51.50000000000000000, -136.0552959530000123 ) ) ;
#20329 = LINE ( 'NONE', #22224, #6780 ) ;
#20330 = CARTESIAN_POINT ( 'NONE',  ( -4.872173186980353066, -28.66560015775754167, -146.5552959530116652 ) ) ;
#20331 = CARTESIAN_POINT ( 'NONE',  ( -7.572469997257414320, 37.05365869149854774, -139.6601318950708048 ) ) ;
#20332 = VERTEX_POINT ( 'NONE', #9687 ) ;
#20333 = CARTESIAN_POINT ( 'NONE',  ( -31.50000000000000000, 14.00000000000000000, -144.0552959529999839 ) ) ;
#20334 = DIRECTION ( 'NONE',  ( -2.909421006506540042E-11, 0.000000000000000000, -1.000000000000000000 ) ) ;
#20335 = CIRCLE ( 'NONE', #16155, 4.000000000000003553 ) ;
#20336 = EDGE_LOOP ( 'NONE', ( #13757, #6382, #8615, #7824 ) ) ;
#20337 = CARTESIAN_POINT ( 'NONE',  ( -31.00000000000000000, -36.00000000000000000, -150.5552959529999839 ) ) ;
#20338 = CARTESIAN_POINT ( 'NONE',  ( -12.36981052416691362, 38.87293897908389084, -148.4153451430249504 ) ) ;
#20339 = DIRECTION ( 'NONE',  ( 2.257144641399999941E-12, -4.009147065140000298E-51, 1.000000000000000000 ) ) ;
#20340 = CARTESIAN_POINT ( 'NONE',  ( -29.54694772409695247, 41.21849320775534409, -145.7548069272761211 ) ) ;
#20341 = EDGE_LOOP ( 'NONE', ( #4394, #5538, #18058 ) ) ;
#20342 = CARTESIAN_POINT ( 'NONE',  ( -32.50000000000000000, 26.00000000000000000, -150.5552959529999839 ) ) ;
#20343 = ORIENTED_EDGE ( 'NONE', *, *, #18711, .F. ) ;
#20344 = DIRECTION ( 'NONE',  ( -1.000000000000000000, 0.000000000000000000, 0.000000000000000000 ) ) ;
#20345 = CARTESIAN_POINT ( 'NONE',  ( -28.42317279839999955, 33.35748734759999934, -144.4144508710000139 ) ) ;
#20346 = EDGE_CURVE ( 'NONE', #576, #12024, #4354, .T. ) ;
#20347 = DIRECTION ( 'NONE',  ( 1.000000000000000000, 0.000000000000000000, 2.516505522483685870E-12 ) ) ;
#20348 = EDGE_CURVE ( 'NONE', #18382, #10837, #2977, .T. ) ;
#20349 = CARTESIAN_POINT ( 'NONE',  ( -21.08990197296929026, 41.23523075628224888, -146.5634232099747578 ) ) ;
#20350 = ORIENTED_EDGE ( 'NONE', *, *, #2461, .F. ) ;
#20351 = DIRECTION ( 'NONE',  ( 1.211690350419999855E-27, 2.765629237170000203E-27, -1.000000000000000000 ) ) ;
#20352 = LINE ( 'NONE', #11401, #4198 ) ;
#20353 = ORIENTED_EDGE ( 'NONE', *, *, #13432, .T. ) ;
#20354 = DIRECTION ( 'NONE',  ( 0.000000000000000000, 1.000000000000000000, 0.000000000000000000 ) ) ;
#20355 = VECTOR ( 'NONE', #20962, 1000.000000000000000 ) ;
#20356 = CARTESIAN_POINT ( 'NONE',  ( -9.157754307290000284, -15.75963164970000108, -147.5552959529999839 ) ) ;
#20357 = CARTESIAN_POINT ( 'NONE',  ( -22.02741209360413777, -4.391489994071226199, -146.3157682190016828 ) ) ;
#20358 = VERTEX_POINT ( 'NONE', #1028 ) ;
#20359 = PLANE ( 'NONE',  #7546 ) ;
#20360 = CARTESIAN_POINT ( 'NONE',  ( 8.100000000049998761, 34.53220746410000430, -148.7552959530000010 ) ) ;
#20361 = VERTEX_POINT ( 'NONE', #16962 ) ;
#20362 = ORIENTED_EDGE ( 'NONE', *, *, #21676, .F. ) ;
#20363 = CARTESIAN_POINT ( 'NONE',  ( -22.79386933271686999, 37.02723109250344891, -140.7029355817511771 ) ) ;
#20364 = CARTESIAN_POINT ( 'NONE',  ( 1.364575185789999923, -21.31553777220000256, -143.0552959529999839 ) ) ;
#20365 = LINE ( 'NONE', #18351, #5219 ) ;
#20366 = CARTESIAN_POINT ( 'NONE',  ( 7.423740471920396544, 35.95513021493444228, -141.7841118834000440 ) ) ;
#20367 = ORIENTED_EDGE ( 'NONE', *, *, #4657, .F. ) ;
#20368 = FILL_AREA_STYLE ('',( #385 ) ) ;
#20369 = AXIS2_PLACEMENT_3D ( 'NONE', #7441, #312, #8984 ) ;
#20370 = CARTESIAN_POINT ( 'NONE',  ( -15.61190926919999988, -1.500000000000000000, -146.8816477750000047 ) ) ;
#20371 = EDGE_CURVE ( 'NONE', #712, #2852, #672, .T. ) ;
#20372 = DIRECTION ( 'NONE',  ( 0.7633862853691524286, 0.6459422414661293299, -5.745404152441152829E-15 ) ) ;
#20373 = DIRECTION ( 'NONE',  ( 2.507771768019999718E-12, 1.592654864209999947E-17, -1.000000000000000000 ) ) ;
#20374 = ADVANCED_FACE ( 'NONE', ( #18987 ), #15185, .F. ) ;
#20375 = CARTESIAN_POINT ( 'NONE',  ( -24.30767937719999949, 40.97374044589999897, -144.4830919949999952 ) ) ;
#20376 = ADVANCED_FACE ( 'NONE', ( #20658 ), #22562, .T. ) ;
#20377 = CARTESIAN_POINT ( 'NONE',  ( -15.24898703719208548, 36.96741147810104167, -148.5896301378323585 ) ) ;
#20378 = CARTESIAN_POINT ( 'NONE',  ( -18.85469010170000459, 37.03971195569999963, -148.4264296979999926 ) ) ;
#20379 = DIRECTION ( 'NONE',  ( 1.000000000000000000, 0.000000000000000000, -4.510774274160000731E-12 ) ) ;
#20380 = LINE ( 'NONE', #8099, #9273 ) ;
#20381 = ORIENTED_EDGE ( 'NONE', *, *, #2912, .T. ) ;
#20382 = CARTESIAN_POINT ( 'NONE',  ( -6.498948513235520252, 40.81543345002808110, -146.1568765785555968 ) ) ;
#20383 = CARTESIAN_POINT ( 'NONE',  ( 22.40884248670000289, -21.39641658300000060, -144.5552959529999839 ) ) ;
#20384 = AXIS2_PLACEMENT_3D ( 'NONE', #15995, #17664, #10151 ) ;
#20385 = AXIS2_PLACEMENT_3D ( 'NONE', #22411, #6106, #4910 ) ;
#20386 = VERTEX_POINT ( 'NONE', #2697 ) ;
#20387 = DIRECTION ( 'NONE',  ( 0.000000000000000000, -1.000000000000000000, -2.245315044999999693E-12 ) ) ;
#20388 = CARTESIAN_POINT ( 'NONE',  ( -23.01751655211429437, 33.66177664240989742, -142.1309265747219115 ) ) ;
#20389 = CARTESIAN_POINT ( 'NONE',  ( 0.3832000607639999834, -34.50000000000000000, -148.5552959529999839 ) ) ;
#20390 = ORIENTED_EDGE ( 'NONE', *, *, #8927, .F. ) ;
#20391 = CARTESIAN_POINT ( 'NONE',  ( -12.63629858846534404, 32.85239007250503107, -143.6876766073750957 ) ) ;
#20392 = CARTESIAN_POINT ( 'NONE',  ( -21.35824191589999899, -4.000000000000000000, -150.0657682190000060 ) ) ;
#20393 = CARTESIAN_POINT ( 'NONE',  ( 13.66051412332252646, 38.90191174487609516, -150.0552959529999839 ) ) ;
#20394 = ITEM_DEFINED_TRANSFORMATION ( 'NONE', 'NONE', #19895,  #5025 ) ;
#20395 = CARTESIAN_POINT ( 'NONE',  ( -2.499999999940000439, 37.00000000000000000, -144.0552959529999839 ) ) ;
#20396 = LINE ( 'NONE', #4091, #600 ) ;
#20397 = LINE ( 'NONE', #12775, #14752 ) ;
#20398 = ORIENTED_EDGE ( 'NONE', *, *, #8041, .F. ) ;
#20399 = AXIS2_PLACEMENT_3D ( 'NONE', #14389, #3567, #5222 ) ;
#20400 = ADVANCED_FACE ( 'NONE', ( #18865 ), #317, .F. ) ;
#20401 = CARTESIAN_POINT ( 'NONE',  ( -28.69387994521298069, 33.30271062198844589, -146.2196849097338429 ) ) ;
#20402 = ORIENTED_EDGE ( 'NONE', *, *, #3025, .F. ) ;
#20403 = ORIENTED_EDGE ( 'NONE', *, *, #9154, .T. ) ;
#20404 = FACE_OUTER_BOUND ( 'NONE', #7243, .T. ) ;
#20405 = DIRECTION ( 'NONE',  ( -0.09606172499277226828, -0.9953753789357124848, 8.265980492677616040E-13 ) ) ;
#20406 = DIRECTION ( 'NONE',  ( 2.257115129720000004E-12, 0.000000000000000000, 1.000000000000000000 ) ) ;
#20407 = ORIENTED_EDGE ( 'NONE', *, *, #4956, .T. ) ;
#20408 = DIRECTION ( 'NONE',  ( -1.000000000000000000, 0.000000000000000000, 0.000000000000000000 ) ) ;
#20409 = ADVANCED_FACE ( 'NONE', ( #17081 ), #4707, .F. ) ;
#20410 = CARTESIAN_POINT ( 'NONE',  ( -4.499999999919999105, 34.00000000000000000, -136.5552959530000123 ) ) ;
#20411 = EDGE_LOOP ( 'NONE', ( #13002, #4729, #12451, #13194, #14956 ) ) ;
#20412 = CARTESIAN_POINT ( 'NONE',  ( -20.76253627919999900, 39.57534689110000414, -140.5049880910000013 ) ) ;
#20413 = AXIS2_PLACEMENT_3D ( 'NONE', #3020, #10366, #21220 ) ;
#20414 = CARTESIAN_POINT ( 'NONE',  ( 9.749519600121018925, 37.82990536602501663, -141.6970570770093047 ) ) ;
#20415 = ADVANCED_FACE ( 'NONE', ( #20902 ), #11949, .F. ) ;
#20416 = DIRECTION ( 'NONE',  ( -1.000000000000000000, -2.602084704489999637E-17, 1.701177084830000066E-20 ) ) ;
#20417 = DIRECTION ( 'NONE',  ( 2.255973186040000320E-12, 0.000000000000000000, 1.000000000000000000 ) ) ;
#20418 = EDGE_LOOP ( 'NONE', ( #10944, #16278, #8416, #14353, #19585, #9603 ) ) ;
#20419 = DIRECTION ( 'NONE',  ( 1.000000000000000000, 0.000000000000000000, -2.259525899719999991E-12 ) ) ;
#20420 = ORIENTED_EDGE ( 'NONE', *, *, #1406, .F. ) ;
#20421 = EDGE_CURVE ( 'NONE', #12346, #8268, #3168, .T. ) ;
#20423 = ORIENTED_EDGE ( 'NONE', *, *, #19869, .T. ) ;
#20422 = AXIS2_PLACEMENT_3D ( 'NONE', #9740, #6196, #13331 ) ;
#20424 = CARTESIAN_POINT ( 'NONE',  ( -26.72208319964573775, 38.71204575040589901, -148.0666639806206035 ) ) ;
#20425 = ORIENTED_EDGE ( 'NONE', *, *, #9522, .T. ) ;
#20426 = CARTESIAN_POINT ( 'NONE',  ( -23.54789306461742626, 36.93722613941654487, -139.7713821669921117 ) ) ;
#20427 = PRESENTATION_LAYER_ASSIGNMENT (  '', '', ( #306 ) ) ;
#20428 = VERTEX_POINT ( 'NONE', #2069 ) ;
#20429 = CYLINDRICAL_SURFACE ( 'NONE', #15203, 5.000000000000000000 ) ;
#20430 = ORIENTED_EDGE ( 'NONE', *, *, #10093, .T. ) ;
#20431 = SHAPE_DEFINITION_REPRESENTATION ( #23266, #15879 ) ;
#20432 = ORIENTED_EDGE ( 'NONE', *, *, #6474, .F. ) ;
#20433 = CARTESIAN_POINT ( 'NONE',  ( -27.05559917085387056, 41.25481893626260899, -146.4757227208741597 ) ) ;
#20434 =( REPRESENTATION_RELATIONSHIP ('NONE','NONE', #7672, #6152 ) REPRESENTATION_RELATIONSHIP_WITH_TRANSFORMATION ( #21725 )SHAPE_REPRESENTATION_RELATIONSHIP( ) );
#20435 = EDGE_CURVE ( 'NONE', #19192, #19834, #8607, .T. ) ;
#20436 = LINE ( 'NONE', #4477, #18610 ) ;
#20437 = CARTESIAN_POINT ( 'NONE',  ( -6.774730888589999722, 51.50000000000000000, -149.5552959529999839 ) ) ;
#20438 = CARTESIAN_POINT ( 'NONE',  ( -5.974012367538351853, 36.93458879463114641, -148.2930816546007122 ) ) ;
#20439 = EDGE_CURVE ( 'NONE', #18780, #17568, #12073, .T. ) ;
#20440 = CARTESIAN_POINT ( 'NONE',  ( 1.133692148550000001, 50.99999999970000175, -136.0552959530000123 ) ) ;
#20441 = FACE_OUTER_BOUND ( 'NONE', #8267, .T. ) ;
#20442 = ORIENTED_EDGE ( 'NONE', *, *, #10432, .F. ) ;
#20443 = PLANE ( 'NONE',  #7173 ) ;
#20444 = AXIS2_PLACEMENT_3D ( 'NONE', #9746, #2524, #11771 ) ;
#20445 = ADVANCED_FACE ( 'NONE', ( #1955 ), #10507, .F. ) ;
#20446 = CARTESIAN_POINT ( 'NONE',  ( 1.713198289069999936, -17.44292009260000142, -147.5552959529999839 ) ) ;
#20447 = EDGE_CURVE ( 'NONE', #19447, #21873, #13609, .T. ) ;
#20448 = CARTESIAN_POINT ( 'NONE',  ( 5.631397321050000571, -17.85059010000000157, -147.5552959529999839 ) ) ;
#20449 = ORIENTED_EDGE ( 'NONE', *, *, #10170, .F. ) ;
#20450 = EDGE_CURVE ( 'NONE', #7723, #15193, #21253, .T. ) ;
#20451 = CARTESIAN_POINT ( 'NONE',  ( -12.16288092095636308, 40.58801103627050821, -142.0245251747066391 ) ) ;
#20452 = ADVANCED_FACE ( 'NONE', ( #12193 ), #9176, .T. ) ;
#20453 = CARTESIAN_POINT ( 'NONE',  ( -17.91974642297896381, 36.92811127467702903, -148.3783205066630444 ) ) ;
#20454 = CARTESIAN_POINT ( 'NONE',  ( 17.58326321919999558, -18.99156222550000095, -147.5552959529999839 ) ) ;
#20455 = ORIENTED_EDGE ( 'NONE', *, *, #16809, .T. ) ;
#20456 = CARTESIAN_POINT ( 'NONE',  ( -6.131111726649999483, 36.14321585209999910, -147.9535578170000178 ) ) ;
#20457 = CARTESIAN_POINT ( 'NONE',  ( -10.01911575600000148, -21.69748113039999637, -147.5552959529999839 ) ) ;
#20458 = ORIENTED_EDGE ( 'NONE', *, *, #8716, .T. ) ;
#20459 = CARTESIAN_POINT ( 'NONE',  ( 12.50000000010000001, 16.89444872450000190, -150.5552959529999839 ) ) ;
#20460 = CARTESIAN_POINT ( 'NONE',  ( 22.36721601470000209, -21.34320095609999868, -148.5552959529999839 ) ) ;
#20461 = ORIENTED_EDGE ( 'NONE', *, *, #12376, .T. ) ;
#20462 = CARTESIAN_POINT ( 'NONE',  ( -3.765581077048879788, 46.49999999999999289, -150.0552959529999839 ) ) ;
#20463 = CARTESIAN_POINT ( 'NONE',  ( -20.26899604979344005, 40.93030953051304266, -143.7497896408696363 ) ) ;
#20464 = VERTEX_POINT ( 'NONE', #6842 ) ;
#20465 = CARTESIAN_POINT ( 'NONE',  ( -26.97085048307042854, 36.11604132840786718, -147.8376774906664366 ) ) ;
#20466 = AXIS2_PLACEMENT_3D ( 'NONE', #11788, #5543, #2217 ) ;
#20467 = LINE ( 'NONE', #5823, #13302 ) ;
#20468 = ORIENTED_EDGE ( 'NONE', *, *, #2859, .T. ) ;
#20469 = CARTESIAN_POINT ( 'NONE',  ( 31.50000000000000000, 0.000000000000000000, -136.0552959530000123 ) ) ;
#20470 = VECTOR ( 'NONE', #16073, 1000.000000000000000 ) ;
#20471 = CARTESIAN_POINT ( 'NONE',  ( 32.50000000000000000, -33.03620104880000241, -136.0552959530000123 ) ) ;
#20472 = DIRECTION ( 'NONE',  ( 1.526468026911764926E-13, 8.159623473496129815E-13, 1.000000000000000000 ) ) ;
#20473 = ORIENTED_EDGE ( 'NONE', *, *, #20704, .T. ) ;
#20474 = CARTESIAN_POINT ( 'NONE',  ( -20.45144833149999997, 36.94873838139999833, -139.8044047869999815 ) ) ;
#20475 = CARTESIAN_POINT ( 'NONE',  ( -2.979194667878099168, 46.44907581354213733, -136.0552959529933048 ) ) ;
#20476 = EDGE_LOOP ( 'NONE', ( #16161, #13708, #8027, #21846 ) ) ;
#20477 = ADVANCED_FACE ( 'NONE', ( #3841 ), #3274, .T. ) ;
#20478 = ORIENTED_EDGE ( 'NONE', *, *, #3251, .T. ) ;
#20479 = FACE_OUTER_BOUND ( 'NONE', #18901, .T. ) ;
#20480 = AXIS2_PLACEMENT_3D ( 'NONE', #15323, #17452, #23050 ) ;
#20481 = LINE ( 'NONE', #20600, #13871 ) ;
#20482 = AXIS2_PLACEMENT_3D ( 'NONE', #1575, #5480, #19884 ) ;
#20483 = CARTESIAN_POINT ( 'NONE',  ( 29.68320006080000084, -32.50000000000000000, -150.0552959529999839 ) ) ;
#20484 = CARTESIAN_POINT ( 'NONE',  ( 31.00000000000000000, 39.80430157320000006, -149.5552959529999839 ) ) ;
#20485 = ORIENTED_EDGE ( 'NONE', *, *, #15929, .F. ) ;
#20486 = LINE ( 'NONE', #7850, #16242 ) ;
#20487 = CARTESIAN_POINT ( 'NONE',  ( -7.628878236750000319, 37.90286001179999431, -140.0026079769999683 ) ) ;
#20488 = CIRCLE ( 'NONE', #3016, 7.499999999999999112 ) ;
#20489 = CARTESIAN_POINT ( 'NONE',  ( 1.561837858109999866, -18.84848306830000197, -143.5552959529999839 ) ) ;
#20490 = CARTESIAN_POINT ( 'NONE',  ( 12.57650987482442595, 37.28094649261360161, -136.0552959530284056 ) ) ;
#20491 = AXIS2_PLACEMENT_3D ( 'NONE', #23078, #13804, #17248 ) ;
#20492 = CARTESIAN_POINT ( 'NONE',  ( -23.64871425658228432, 39.79993930545538916, -140.2199279868687256 ) ) ;
#20493 = CARTESIAN_POINT ( 'NONE',  ( -15.07147389515268721, 36.94622240755791864, -147.6034838243276113 ) ) ;
#20494 = CARTESIAN_POINT ( 'NONE',  ( -16.13502618060000060, 32.80445174449999968, -146.2787800969999807 ) ) ;
#20495 = CARTESIAN_POINT ( 'NONE',  ( -5.070907855429999778, -22.41528233759999722, -147.5552959529999839 ) ) ;
#20496 = CARTESIAN_POINT ( 'NONE',  ( 16.26251912989999937, -22.62374141290000296, -144.5552959529999839 ) ) ;
#20497 = LINE ( 'NONE', #4197, #20305 ) ;
#20498 = VECTOR ( 'NONE', #5056, 1000.000000000000000 ) ;
#20499 = ORIENTED_EDGE ( 'NONE', *, *, #13915, .F. ) ;
#20500 = CARTESIAN_POINT ( 'NONE',  ( -5.844227446867898301, 38.54059235905305059, -140.3554711806842477 ) ) ;
#20501 = DIRECTION ( 'NONE',  ( 0.000000000000000000, 1.000000000000000000, 0.000000000000000000 ) ) ;
#20502 = VECTOR ( 'NONE', #10590, 1000.000000000000000 ) ;
#20503 = ORIENTED_EDGE ( 'NONE', *, *, #20826, .T. ) ;
#20504 = CARTESIAN_POINT ( 'NONE',  ( -1.499999999969999998, 44.50000000000000000, -137.0552959530000123 ) ) ;
#20505 = VECTOR ( 'NONE', #12550, 1000.000000000000000 ) ;
#20506 = ADVANCED_FACE ( 'NONE', ( #6719 ), #19468, .F. ) ;
#20507 = VECTOR ( 'NONE', #22882, 1000.000000000000000 ) ;
#20508 = CARTESIAN_POINT ( 'NONE',  ( -22.56645868524751464, 33.58406826459463446, -146.0350363999489502 ) ) ;
#20509 = CARTESIAN_POINT ( 'NONE',  ( 5.276897646260000130, -21.39828525539999760, -144.5552959529999839 ) ) ;
#20510 = VERTEX_POINT ( 'NONE', #23268 ) ;
#20511 = CARTESIAN_POINT ( 'NONE',  ( -12.21344923919432546, 35.51569570616177174, -147.3850191185591143 ) ) ;
#20512 = CARTESIAN_POINT ( 'NONE',  ( -16.45586251407963729, 37.06757768449541146, -140.3467090679219780 ) ) ;
#20513 = DIRECTION ( 'NONE',  ( 0.000000000000000000, 1.000000000000000000, 0.000000000000000000 ) ) ;
#20514 = LINE ( 'NONE', #4329, #2112 ) ;
#20515 = AXIS2_PLACEMENT_3D ( 'NONE', #1762, #23171, #18051 ) ;
#20516 = CARTESIAN_POINT ( 'NONE',  ( 3.038050104604336887, -3.890583939891920640, -136.0552959530068904 ) ) ;
#20517 = ORIENTED_EDGE ( 'NONE', *, *, #6361, .F. ) ;
#20518 = VECTOR ( 'NONE', #21591, 1000.000000000000000 ) ;
#20519 = VECTOR ( 'NONE', #11786, 1000.000000000000000 ) ;
#20520 = DIRECTION ( 'NONE',  ( 0.000000000000000000, 0.000000000000000000, 1.000000000000000000 ) ) ;
#20521 = AXIS2_PLACEMENT_3D ( 'NONE', #2959, #13788, #4738 ) ;
#20522 = CIRCLE ( 'NONE', #8345, 15.00000000000000000 ) ;
#20523 = ORIENTED_EDGE ( 'NONE', *, *, #21074, .F. ) ;
#20524 = CARTESIAN_POINT ( 'NONE',  ( -12.87353035906786047, 34.29620811505558464, -147.9524828210263934 ) ) ;
#20525 = CARTESIAN_POINT ( 'NONE',  ( 31.00000000000000000, 39.80430157320000006, -151.0552959529999839 ) ) ;
#20526 = DIRECTION ( 'NONE',  ( 3.882490197650000213E-51, -1.000000000000000000, -4.009147065150000317E-51 ) ) ;
#20527 = VERTEX_POINT ( 'NONE', #20025 ) ;
#20528 = CARTESIAN_POINT ( 'NONE',  ( -4.499999999949999996, 42.50000000000000000, -150.0552959529999839 ) ) ;
#20529 = CARTESIAN_POINT ( 'NONE',  ( 8.100000000049998761, 34.53220746410000430, -149.1552959530000066 ) ) ;
#20530 = VERTEX_POINT ( 'NONE', #18358 ) ;
#20531 = CARTESIAN_POINT ( 'NONE',  ( -20.61753010269738340, 36.92891383027765784, -140.0927360959155976 ) ) ;
#20532 = ADVANCED_FACE ( 'NONE', ( #14105 ), #22279, .F. ) ;
#20533 = CARTESIAN_POINT ( 'NONE',  ( 9.649788648777766653, 37.96362004170691762, -141.7484567676849281 ) ) ;
#20534 = EDGE_CURVE ( 'NONE', #20624, #7366, #16801, .T. ) ;
#20535 = VECTOR ( 'NONE', #18555, 1000.000000000000000 ) ;
#20536 = VECTOR ( 'NONE', #18745, 999.9999999999998863 ) ;
#20537 = CARTESIAN_POINT ( 'NONE',  ( -3.499999999969999998, 42.50000000000000000, -137.0552959530000123 ) ) ;
#20538 = CYLINDRICAL_SURFACE ( 'NONE', #14329, 0.5000000000000079936 ) ;
#20539 = EDGE_LOOP ( 'NONE', ( #4780, #15644, #16970, #17611 ) ) ;
#20540 = CARTESIAN_POINT ( 'NONE',  ( 19.84954298779999959, -51.20423285649999912, -149.5552959529999839 ) ) ;
#20541 = ORIENTED_EDGE ( 'NONE', *, *, #10532, .F. ) ;
#20542 = CARTESIAN_POINT ( 'NONE',  ( 7.014880255698754397, -48.99993274156953049, -150.0552959529999839 ) ) ;
#20543 = ADVANCED_FACE ( 'NONE', ( #6089 ), #623, .F. ) ;
#20544 = ORIENTED_EDGE ( 'NONE', *, *, #10004, .F. ) ;
#20545 = ORIENTED_EDGE ( 'NONE', *, *, #17238, .F. ) ;
#20546 = CARTESIAN_POINT ( 'NONE',  ( 22.36721601470000209, -21.34320095609999868, -148.0552959529999839 ) ) ;
#20547 = ORIENTED_EDGE ( 'NONE', *, *, #20297, .T. ) ;
#20548 = LINE ( 'NONE', #11483, #9105 ) ;
#20549 = VERTEX_POINT ( 'NONE', #13451 ) ;
#20550 = CIRCLE ( 'NONE', #12573, 1.000000000000000888 ) ;
#20551 = EDGE_CURVE ( 'NONE', #5119, #4448, #2526, .T. ) ;
#20552 = ORIENTED_EDGE ( 'NONE', *, *, #10246, .F. ) ;
#20553 = CARTESIAN_POINT ( 'NONE',  ( -10.00000000000000000, 42.50000000000000000, -150.0552959529999839 ) ) ;
#20554 = CARTESIAN_POINT ( 'NONE',  ( -21.35824191589999899, -32.00000000000000000, -144.8157682190000060 ) ) ;
#20555 = CARTESIAN_POINT ( 'NONE',  ( 24.38136133040000075, -29.22855050349999928, -145.5552959529999839 ) ) ;
#20556 = DIRECTION ( 'NONE',  ( 0.000000000000000000, 0.000000000000000000, 1.000000000000000000 ) ) ;
#20557 = CARTESIAN_POINT ( 'NONE',  ( -6.663373516737825852, 36.04829920608432303, -148.7421194615091906 ) ) ;
#20558 = CARTESIAN_POINT ( 'NONE',  ( -8.098664391214354552, 41.05008105453497080, -141.7339891042810223 ) ) ;
#20559 = ORIENTED_EDGE ( 'NONE', *, *, #16787, .T. ) ;
#20560 = CARTESIAN_POINT ( 'NONE',  ( -1.898424454315990273, 45.72687021304480481, -150.0552959530000123 ) ) ;
#20561 = EDGE_CURVE ( 'NONE', #18664, #546, #5643, .T. ) ;
#20562 = CARTESIAN_POINT ( 'NONE',  ( 9.843499027571208870, 37.67425020617515941, -146.4644491674870324 ) ) ;
#20563 = LINE ( 'NONE', #9477, #1897 ) ;
#20564 = AXIS2_PLACEMENT_3D ( 'NONE', #16153, #19846, #1185 ) ;
#20565 = ORIENTED_EDGE ( 'NONE', *, *, #1853, .T. ) ;
#20566 = MECHANICAL_DESIGN_GEOMETRIC_PRESENTATION_REPRESENTATION (  '', ( #22097 ), #16393 ) ;
#20567 = CARTESIAN_POINT ( 'NONE',  ( -12.18519546026979050, 41.69055574765604177, -144.6655014886106017 ) ) ;
#20568 = EDGE_CURVE ( 'NONE', #13256, #2055, #17379, .T. ) ;
#20569 = PLANE ( 'NONE',  #19664 ) ;
#20570 = CARTESIAN_POINT ( 'NONE',  ( -23.22224815339999893, 34.57381638260000045, -140.7548632179999970 ) ) ;
#20571 = ORIENTED_EDGE ( 'NONE', *, *, #99, .F. ) ;
#20572 = CARTESIAN_POINT ( 'NONE',  ( -7.529689113779999943, 37.05876528330000497, -139.9906690790000141 ) ) ;
#20573 = CARTESIAN_POINT ( 'NONE',  ( -31.00000000000000000, 19.50000000000000000, -150.0552959529999839 ) ) ;
#20574 = ORIENTED_EDGE ( 'NONE', *, *, #1371, .F. ) ;
#20575 = LINE ( 'NONE', #2731, #15 ) ;
#20576 = DIRECTION ( 'NONE',  ( -8.955190032050000935E-12, 9.104778821549999739E-13, -1.000000000000000000 ) ) ;
#20577 = ORIENTED_EDGE ( 'NONE', *, *, #16399, .T. ) ;
#20578 = CARTESIAN_POINT ( 'NONE',  ( -4.726870213046807656, 46.10157554568340288, -150.0552959529999839 ) ) ;
#20579 = CARTESIAN_POINT ( 'NONE',  ( -19.49482955066354606, 37.94579615576876108, -139.9758014792360541 ) ) ;
#20580 = ORIENTED_EDGE ( 'NONE', *, *, #11857, .F. ) ;
#20581 = DIRECTION ( 'NONE',  ( 1.000000000000000000, 0.000000000000000000, -2.259525899719999991E-12 ) ) ;
#20582 = EDGE_CURVE ( 'NONE', #17829, #13267, #2764, .T. ) ;
#20583 = DIRECTION ( 'NONE',  ( 2.257144641399999941E-12, -8.049635416090000264E-35, 1.000000000000000000 ) ) ;
#20584 = EDGE_LOOP ( 'NONE', ( #3598, #18642 ) ) ;
#20585 = DIRECTION ( 'NONE',  ( 2.257144641399999941E-12, -8.049736840714550138E-35, 1.000000000000000000 ) ) ;
#20586 = EDGE_CURVE ( 'NONE', #19967, #18273, #20838, .T. ) ;
#20587 = CARTESIAN_POINT ( 'NONE',  ( -21.35824191589999899, -32.00000000000000000, -144.8157682190000060 ) ) ;
#20588 = VECTOR ( 'NONE', #21082, 1000.000000000000000 ) ;
#20589 = CARTESIAN_POINT ( 'NONE',  ( -22.10824191589999899, -4.000000000000000000, -146.3157682190000060 ) ) ;
#20590 = CLOSED_SHELL ( 'NONE', ( #12248, #8531, #21538, #17990, #22621, #5157, #7293, #8031, #7892, #6231, #21910, #8437, #3935, #16601, #3150, #11660, #11484, #18593, #13483, #13235, #14921, #16290, #8077, #8789, #5855, #1765, #4701, #19240, #11035, #18399, #12001, #11849, #11407, #12455, #1407, #8495, #15935, #6303, #6343, #23300, #640, #7052, #17815, #7776, #7316, #18849, #13327, #13418, #7648, #16374, #14336, #172, #14449, #12714, #18514, #827, #22906, #23223, #11343, #6183, #17634, #10706, #256 ) ) ;
#20591 = VECTOR ( 'NONE', #4072, 1000.000000000000000 ) ;
#20592 = EDGE_CURVE ( 'NONE', #20668, #15779, #5274, .T. ) ;
#20593 = ORIENTED_EDGE ( 'NONE', *, *, #19971, .T. ) ;
#20594 = CARTESIAN_POINT ( 'NONE',  ( 11.48351823926500437, -19.88604765140169661, -148.5552959529999839 ) ) ;
#20595 = EDGE_CURVE ( 'NONE', #9931, #19743, #2872, .T. ) ;
#20596 = CARTESIAN_POINT ( 'NONE',  ( -16.30974947700681810, -43.75752630172158320, -136.0552959529631778 ) ) ;
#20597 = ORIENTED_EDGE ( 'NONE', *, *, #9302, .F. ) ;
#20598 = VERTEX_POINT ( 'NONE', #11773 ) ;
#20599 = CARTESIAN_POINT ( 'NONE',  ( -23.11170852288484667, 36.28661503646119257, -140.7058601757693737 ) ) ;
#20600 = CARTESIAN_POINT ( 'NONE',  ( 25.00000852249999994, -26.83294714660000224, -143.0552959529999839 ) ) ;
#20601 = CARTESIAN_POINT ( 'NONE',  ( -2.499999999940000439, 34.80604359529999670, -142.8567321060000097 ) ) ;
#20602 = CARTESIAN_POINT ( 'NONE',  ( 7.366555212978977529, 36.01714620922514598, -141.7565619021944485 ) ) ;
#20603 = ORIENTED_EDGE ( 'NONE', *, *, #13727, .T. ) ;
#20604 = PRESENTATION_STYLE_ASSIGNMENT (( #15120 ) ) ;
#20605 = VECTOR ( 'NONE', #12959, 999.9999999999998863 ) ;
#20606 = VECTOR ( 'NONE', #10608, 1000.000000000000000 ) ;
#20607 = CARTESIAN_POINT ( 'NONE',  ( -13.86630785140000022, -51.50000000000000000, -137.0552959530000123 ) ) ;
#20608 = EDGE_CURVE ( 'NONE', #2844, #13263, #13565, .T. ) ;
#20609 = VECTOR ( 'NONE', #22369, 1000.000000000000000 ) ;
#20610 = B_SPLINE_CURVE_WITH_KNOTS ( 'NONE', 1,
 ( #7203, #7321 ),
 .UNSPECIFIED., .F., .F.,
 ( 2, 2 ),
 ( -0.5146970993560000540, 15.26952906260000020 ),
 .UNSPECIFIED. ) ;
#20611 = CARTESIAN_POINT ( 'NONE',  ( -9.434278515689999978, -18.41834002140000237, -147.5552959529999839 ) ) ;
#20612 = FACE_OUTER_BOUND ( 'NONE', #20271, .T. ) ;
#20613 = CARTESIAN_POINT ( 'NONE',  ( -23.72311861867038729, 41.82577330078812849, -143.6112047735845181 ) ) ;
#20614 = CARTESIAN_POINT ( 'NONE',  ( -15.15646599586469634, 34.44462052388409745, -147.2304959536884894 ) ) ;
#20615 = EDGE_CURVE ( 'NONE', #15302, #11614, #7158, .T. ) ;
#20616 = CARTESIAN_POINT ( 'NONE',  ( -17.49915212496940953, 35.33646836210735387, -140.3085081534657093 ) ) ;
#20617 = ADVANCED_FACE ( 'NONE', ( #8206 ), #15717, .T. ) ;
#20618 = CARTESIAN_POINT ( 'NONE',  ( -19.14968637899999848, 34.49201595030000078, -147.7870032629999741 ) ) ;
#20619 = DIRECTION ( 'NONE',  ( 0.000000000000000000, 2.259525899719999991E-12, 1.000000000000000000 ) ) ;
#20620 = DIRECTION ( 'NONE',  ( 1.526468026912475027E-13, 8.159623473505000399E-13, 1.000000000000000000 ) ) ;
#20621 = ORIENTED_EDGE ( 'NONE', *, *, #14724, .F. ) ;
#20622 = DIRECTION ( 'NONE',  ( 2.507554887169999917E-12, 0.000000000000000000, -1.000000000000000000 ) ) ;
#20623 = FACE_BOUND ( 'NONE', #3252, .T. ) ;
#20624 = VERTEX_POINT ( 'NONE', #12135 ) ;
#20625 = CONICAL_SURFACE ( 'NONE', #14912, 1.999999999999995115, 0.7853981633970000820 ) ;
#20626 =( NAMED_UNIT ( * ) PLANE_ANGLE_UNIT ( ) SI_UNIT ( $, .RADIAN. ) );
#20627 = CARTESIAN_POINT ( 'NONE',  ( -22.11386115772126004, 33.57646858666087297, -144.3495254905444085 ) ) ;
#20628 = DIRECTION ( 'NONE',  ( -1.527666881879999979E-13, -8.171241461240000022E-13, -1.000000000000000000 ) ) ;
#20629 = VERTEX_POINT ( 'NONE', #10347 ) ;
#20630 = CARTESIAN_POINT ( 'NONE',  ( -12.91608596194663861, 33.62894392469238625, -142.1625766469311429 ) ) ;
#20631 = CARTESIAN_POINT ( 'NONE',  ( 4.499999999879999102, -2.000000000000000000, -143.0552959529999839 ) ) ;
#20632 = CARTESIAN_POINT ( 'NONE',  ( -34.35824191590000254, -34.50000000000000000, -150.0657682190000060 ) ) ;
#20633 = CONTEXT_DEPENDENT_SHAPE_REPRESENTATION ( #12816, #17333 ) ;
#20634 = CARTESIAN_POINT ( 'NONE',  ( -6.657076963140000636, -20.13603737529999904, -145.5552959529999839 ) ) ;
#20635 = DIRECTION ( 'NONE',  ( 1.211690350419999855E-27, 2.765629237170000203E-27, -1.000000000000000000 ) ) ;
#20636 = CARTESIAN_POINT ( 'NONE',  ( -7.695630400395947923, 37.03895750127035313, -140.6427397355593030 ) ) ;
#20637 = EDGE_LOOP ( 'NONE', ( #16647, #9784, #3304, #23149, #20675, #16033 ) ) ;
#20638 = STYLED_ITEM ( 'NONE', ( #13958 ), #1875 ) ;
#20639 = CARTESIAN_POINT ( 'NONE',  ( 8.750000000000000000, 0.000000000000000000, -150.0552959529999839 ) ) ;
#20640 = EDGE_CURVE ( 'NONE', #14365, #4754, #17266, .T. ) ;
#20641 = EDGE_CURVE ( 'NONE', #18669, #2618, #10230, .T. ) ;
#20642 = VERTEX_POINT ( 'NONE', #15475 ) ;
#20643 = CARTESIAN_POINT ( 'NONE',  ( -14.70358821728447474, 36.91864139954388691, -140.0875527723345897 ) ) ;
#20644 = DIRECTION ( 'NONE',  ( 0.7633862853691524286, -0.6459422414661293299, 2.886579864030576411E-15 ) ) ;
#20645 = DIRECTION ( 'NONE',  ( -1.000000000000000000, 0.000000000000000000, 0.000000000000000000 ) ) ;
#20646 = EDGE_LOOP ( 'NONE', ( #20655, #557, #20064, #17279 ) ) ;
#20647 = CARTESIAN_POINT ( 'NONE',  ( 11.68320006079999906, -20.50000000000000000, -149.3052959529999839 ) ) ;
#20648 = CARTESIAN_POINT ( 'NONE',  ( -32.50000000000000000, 47.50000000000000000, -150.0552959529999839 ) ) ;
#20649 = ORIENTED_EDGE ( 'NONE', *, *, #13104, .T. ) ;
#20650 = CARTESIAN_POINT ( 'NONE',  ( 11.10910039985186160, 14.50249868201364656, -136.0552959530104147 ) ) ;
#20651 = CARTESIAN_POINT ( 'NONE',  ( 9.291372094100973200, 38.27544467346150014, -141.9048323916335050 ) ) ;
#20652 = DIRECTION ( 'NONE',  ( 1.000000000000000000, 0.000000000000000000, -2.257144641399999941E-12 ) ) ;
#20653 = CARTESIAN_POINT ( 'NONE',  ( -23.48449349015688270, 36.94479390616783832, -140.4349842069358090 ) ) ;
#20654 = CARTESIAN_POINT ( 'NONE',  ( -25.46021907539999773, 33.59345108530000346, -146.1038275270000213 ) ) ;
#20655 = ORIENTED_EDGE ( 'NONE', *, *, #3938, .T. ) ;
#20656 = CARTESIAN_POINT ( 'NONE',  ( -34.50000000000000000, 46.00000000000000000, -144.0552959529999839 ) ) ;
#20657 = VERTEX_POINT ( 'NONE', #4771 ) ;
#20658 = FACE_OUTER_BOUND ( 'NONE', #8939, .T. ) ;
#20659 = EDGE_CURVE ( 'NONE', #3396, #17827, #19529, .T. ) ;
#20660 = VERTEX_POINT ( 'NONE', #19283 ) ;
#20661 = ORIENTED_EDGE ( 'NONE', *, *, #19317, .T. ) ;
#20662 = EDGE_CURVE ( 'NONE', #6145, #12329, #19050, .T. ) ;
#20663 = DIRECTION ( 'NONE',  ( 2.257305453670000045E-12, 0.000000000000000000, 1.000000000000000000 ) ) ;
#20664 = EDGE_LOOP ( 'NONE', ( #1541, #21155 ) ) ;
#20665 = DIRECTION ( 'NONE',  ( 1.000000000000000000, 0.000000000000000000, -2.259303855112193560E-12 ) ) ;
#20666 = EDGE_CURVE ( 'NONE', #8429, #2933, #17500, .T. ) ;
#20667 = ORIENTED_EDGE ( 'NONE', *, *, #1278, .F. ) ;
#20668 = VERTEX_POINT ( 'NONE', #21317 ) ;
#20669 = CARTESIAN_POINT ( 'NONE',  ( -27.68847005644245129, 39.80069049611315535, -147.7731842270326581 ) ) ;
#20670 = LINE ( 'NONE', #570, #20897 ) ;
#20671 = CARTESIAN_POINT ( 'NONE',  ( -21.71608528380000180, -34.50000000000000000, -146.3157682190000060 ) ) ;
#20672 = CARTESIAN_POINT ( 'NONE',  ( -4.499999999929999994, 32.75000000000000000, -138.0552959530000123 ) ) ;
#20673 = CARTESIAN_POINT ( 'NONE',  ( -30.49999999990000177, 26.50000000000000000, -140.5552959529999839 ) ) ;
#20674 = CARTESIAN_POINT ( 'NONE',  ( 32.50000000000000000, 36.50000000010000178, -136.0552959530000123 ) ) ;
#20675 = ORIENTED_EDGE ( 'NONE', *, *, #10283, .F. ) ;
#20676 = DIRECTION ( 'NONE',  ( -0.09606172499277226828, -0.9953753789357124848, 8.289665250527615055E-13 ) ) ;
#20677 = DIRECTION ( 'NONE',  ( 1.000000000000000000, 0.000000000000000000, 0.000000000000000000 ) ) ;
#20678 = DIRECTION ( 'NONE',  ( 0.9848077530125619594, 0.000000000000000000, 0.1736481776649230202 ) ) ;
#20679 = VERTEX_POINT ( 'NONE', #9989 ) ;
#20680 = AXIS2_PLACEMENT_3D ( 'NONE', #164, #18364, #3370 ) ;
#20681 = CARTESIAN_POINT ( 'NONE',  ( -18.31895680040000229, 41.06933176500000116, -146.2870363079999834 ) ) ;
#20682 = DIRECTION ( 'NONE',  ( 0.000000000000000000, 0.000000000000000000, -1.000000000000000000 ) ) ;
#20683 = ORIENTED_EDGE ( 'NONE', *, *, #17277, .T. ) ;
#20684 = CARTESIAN_POINT ( 'NONE',  ( 16.25412235410000150, -22.59491385829999999, -146.5552959529999839 ) ) ;
#20685 = DIRECTION ( 'NONE',  ( 1.526468026909999897E-13, 8.159623473500000156E-13, 1.000000000000000000 ) ) ;
#20686 = ORIENTED_EDGE ( 'NONE', *, *, #21184, .F. ) ;
#20687 = CARTESIAN_POINT ( 'NONE',  ( -31.00000000000000000, 37.00000000000000000, -149.5552959529999839 ) ) ;
#20688 = CARTESIAN_POINT ( 'NONE',  ( 20.50000000000000000, -20.50000000000000000, -150.0552959529999839 ) ) ;
#20689 = ORIENTED_EDGE ( 'NONE', *, *, #6586, .T. ) ;
#20690 = LINE ( 'NONE', #18330, #7903 ) ;
#20691 = CARTESIAN_POINT ( 'NONE',  ( -21.53332179724142748, 37.97490292932302935, -148.7165867017075982 ) ) ;
#20692 = EDGE_CURVE ( 'NONE', #21589, #4899, #5008, .T. ) ;
#20693 = ORIENTED_EDGE ( 'NONE', *, *, #8203, .F. ) ;
#20694 =( NAMED_UNIT ( * ) SI_UNIT ( $, .STERADIAN. ) SOLID_ANGLE_UNIT ( ) );
#20695 = CARTESIAN_POINT ( 'NONE',  ( -28.62185635698285324, 35.60280024164048029, -140.7936020328396296 ) ) ;
#20696 = CARTESIAN_POINT ( 'NONE',  ( 8.750000000000000000, -47.00000000000000000, -151.0552959529999839 ) ) ;
#20697 = VERTEX_POINT ( 'NONE', #6314 ) ;
#20698 = DIRECTION ( 'NONE',  ( 8.955190032050000935E-12, -9.104778821549999739E-13, 1.000000000000000000 ) ) ;
#20699 = CARTESIAN_POINT ( 'NONE',  ( 8.915010983423528046, -17.39036197557994612, -144.5552959530300257 ) ) ;
#20700 = VERTEX_POINT ( 'NONE', #1095 ) ;
#20701 = CARTESIAN_POINT ( 'NONE',  ( -11.29029698189999920, 36.23043332049999776, -140.4049246349999862 ) ) ;
#20702 = ORIENTED_EDGE ( 'NONE', *, *, #17554, .T. ) ;
#20703 = LINE ( 'NONE', #15351, #16676 ) ;
#20704 = EDGE_CURVE ( 'NONE', #2624, #6475, #20966, .T. ) ;
#20705 = CARTESIAN_POINT ( 'NONE',  ( -16.49999999999998579, -43.19923223293173464, -136.0552959529627515 ) ) ;
#20706 = ORIENTED_EDGE ( 'NONE', *, *, #21019, .T. ) ;
#20707 = ORIENTED_EDGE ( 'NONE', *, *, #5153, .F. ) ;
#20708 = CARTESIAN_POINT ( 'NONE',  ( 2.100999472805455959, -1.656359840075259937, -150.0552959529999839 ) ) ;
#20709 = EDGE_CURVE ( 'NONE', #941, #9252, #10106, .T. ) ;
#20710 = DIRECTION ( 'NONE',  ( -2.423380700840000070E-27, 0.000000000000000000, -1.000000000000000000 ) ) ;
#20711 = CARTESIAN_POINT ( 'NONE',  ( 14.25179003943139655, -18.18074738980093130, -145.5552959530190833 ) ) ;
#20712 = CARTESIAN_POINT ( 'NONE',  ( 20.40453940470000305, -31.75469340779999428, -144.5552959529999839 ) ) ;
#20713 = EDGE_LOOP ( 'NONE', ( #2187, #19692, #17184, #12425 ) ) ;
#20714 = FACE_OUTER_BOUND ( 'NONE', #3852, .T. ) ;
#20715 = LINE ( 'NONE', #17143, #7041 ) ;
#20716 = EDGE_CURVE ( 'NONE', #21412, #16256, #5363, .T. ) ;
#20717 = CARTESIAN_POINT ( 'NONE',  ( -13.79923503141243302, -42.08020845437312829, -150.0552959529999839 ) ) ;
#20718 = DIRECTION ( 'NONE',  ( -1.000000000000000000, 0.000000000000000000, 0.000000000000000000 ) ) ;
#20719 = CARTESIAN_POINT ( 'NONE',  ( -24.02064066296885514, 38.85110534163130325, -148.3889946021463970 ) ) ;
#20720 = VECTOR ( 'NONE', #16061, 1000.000000000000227 ) ;
#20721 = DIRECTION ( 'NONE',  ( 1.000000000000000000, 0.000000000000000000, 0.000000000000000000 ) ) ;
#20722 = DIRECTION ( 'NONE',  ( 0.000000000000000000, 0.000000000000000000, -1.000000000000000000 ) ) ;
#20723 = MECHANICAL_DESIGN_GEOMETRIC_PRESENTATION_REPRESENTATION (  '', ( #209 ), #19963 ) ;
#20724 = DIRECTION ( 'NONE',  ( 1.000000000000000000, 0.000000000000000000, 2.516505522483685870E-12 ) ) ;
#20725 = CARTESIAN_POINT ( 'NONE',  ( 18.95053822279999878, -51.00000000000000000, -149.5552959529999839 ) ) ;
#20726 = DIRECTION ( 'NONE',  ( 0.000000000000000000, 1.000000000000000000, 0.000000000000000000 ) ) ;
#20727 = ORIENTED_EDGE ( 'NONE', *, *, #15369, .T. ) ;
#20728 = CARTESIAN_POINT ( 'NONE',  ( -10.07619956199374123, 36.21908991350156271, -147.8536995445676041 ) ) ;
#20729 = CARTESIAN_POINT ( 'NONE',  ( 31.50000000000000000, 40.03620104880000241, -136.0552959530000123 ) ) ;
#20730 = EDGE_CURVE ( 'NONE', #9450, #8748, #12837, .T. ) ;
#20731 = LINE ( 'NONE', #16715, #17789 ) ;
#20732 = ORIENTED_EDGE ( 'NONE', *, *, #22197, .F. ) ;
#20733 = ADVANCED_FACE ( 'NONE', ( #16189 ), #15952, .T. ) ;
#20734 =( NAMED_UNIT ( * ) PLANE_ANGLE_UNIT ( ) SI_UNIT ( $, .RADIAN. ) );
#20736 = AXIS2_PLACEMENT_3D ( 'NONE', #6310, #507, #2638 ) ;
#20735 = LINE ( 'NONE', #5858, #5168 ) ;
#20737 = CIRCLE ( 'NONE', #19603, 10.00000000000000000 ) ;
#20738 = LINE ( 'NONE', #6330, #7572 ) ;
#20739 = ORIENTED_EDGE ( 'NONE', *, *, #2514, .F. ) ;
#20740 = CARTESIAN_POINT ( 'NONE',  ( -22.62924774403715844, 37.91877106620272286, -140.0196664478621926 ) ) ;
#20741 = EDGE_CURVE ( 'NONE', #18313, #19961, #1862, .T. ) ;
#20742 = CARTESIAN_POINT ( 'NONE',  ( -25.86630785129999666, -51.00000000000000000, -136.0552959530000123 ) ) ;
#20743 = EDGE_CURVE ( 'NONE', #1513, #1364, #136, .T. ) ;
#20744 = CYLINDRICAL_SURFACE ( 'NONE', #19268, 8.176568160359998672 ) ;
#20745 = FACE_OUTER_BOUND ( 'NONE', #12586, .T. ) ;
#20746 = LINE ( 'NONE', #4212, #11269 ) ;
#20747 = CARTESIAN_POINT ( 'NONE',  ( -8.296392858609999976, -9.821782169089999570, -147.5552959529999839 ) ) ;
#20748 = ADVANCED_FACE ( 'NONE', ( #21678 ), #3693, .T. ) ;
#20749 = CARTESIAN_POINT ( 'NONE',  ( -8.031950161270000166, 40.75709267670000457, -141.9144354160000034 ) ) ;
#20750 = EDGE_CURVE ( 'NONE', #5196, #10172, #12609, .T. ) ;
#20751 = VERTEX_POINT ( 'NONE', #10570 ) ;
#20752 =( BOUNDED_SURFACE ( )  B_SPLINE_SURFACE ( 5, 5, ( 
 ( #6507, #6264, #8272, #11844, #10300, #22810 ),
 ( #18877, #21150, #13514, #2590, #20788, #21031 ),
 ( #13771, #4720, #11963, #19228, #10175, #4478 ),
 ( #22937, #2712, #9816, #17576, #1290, #15782 ),
 ( #17094, #17209, #812, #11721, #8151, #13992 ),
 ( #16142, #18159, #5184, #19595, #9094, #5431 ),
 ( #10760, #1520, #19708, #23515, #18043, #1394 ),
 ( #7212, #3530, #23283, #3288, #23396, #4961 ),
 ( #19944, #10412, #1871, #21265, #21389, #8620 ),
 ( #10643, #23045, #17926, #8863, #6973, #5075 ),
 ( #14121, #12434, #21743, #7092, #14351, #14474 ),
 ( #21623, #1754, #19832, #12676, #5305, #10879 ) ),
 .UNSPECIFIED., .F., .F., .F. ) 
 B_SPLINE_SURFACE_WITH_KNOTS ( ( 6, 3, 3, 6 ),
 ( 6, 6 ),
 ( 0.000000000000000000, 4.398006073320000375, 8.633600727160001043, 12.71824907600000110 ),
 ( 0.000000000000000000, 1.570796326852889946 ),
 .UNSPECIFIED. ) 
 GEOMETRIC_REPRESENTATION_ITEM ( )  RATIONAL_B_SPLINE_SURFACE ( (
 ( 1.000000000000000000, 0.5999999999852579924, 0.3999999999852579813, 0.2999999999889434998, 0.2499999999926290073, 0.2500000000000000000),
 ( 1.000000000000000000, 0.5999999999852579924, 0.3999999999852579813, 0.2999999999889434998, 0.2499999999926290073, 0.2500000000000000000),
 ( 1.000000000000000000, 0.5999999999852579924, 0.3999999999852579813, 0.2999999999889434998, 0.2499999999926290073, 0.2500000000000000000),
 ( 1.000000000000000000, 0.5999999999852579924, 0.3999999999852579813, 0.2999999999889434998, 0.2499999999926290073, 0.2500000000000000000),
 ( 1.000000000000000000, 0.5999999999852579924, 0.3999999999852579813, 0.2999999999889434998, 0.2499999999926290073, 0.2500000000000000000),
 ( 1.000000000000000000, 0.5999999999852579924, 0.3999999999852579813, 0.2999999999889434998, 0.2499999999926290073, 0.2500000000000000000),
 ( 1.000000000000000000, 0.5999999999852579924, 0.3999999999852579813, 0.2999999999889434998, 0.2499999999926290073, 0.2500000000000000000),
 ( 1.000000000000000000, 0.5999999999852579924, 0.3999999999852579813, 0.2999999999889434998, 0.2499999999926290073, 0.2500000000000000000),
 ( 1.000000000000000000, 0.5999999999852579924, 0.3999999999852579813, 0.2999999999889434998, 0.2499999999926290073, 0.2500000000000000000),
 ( 1.000000000000000000, 0.5999999999852579924, 0.3999999999852579813, 0.2999999999889434998, 0.2499999999926290073, 0.2500000000000000000),
 ( 1.000000000000000000, 0.5999999999852579924, 0.3999999999852579813, 0.2999999999889434998, 0.2499999999926290073, 0.2500000000000000000),
 ( 1.000000000000000000, 0.5999999999852579924, 0.3999999999852579813, 0.2999999999889434998, 0.2499999999926290073, 0.2500000000000000000) ) ) 
 REPRESENTATION_ITEM ( '' )  SURFACE ( )  );
#20753 = CARTESIAN_POINT ( 'NONE',  ( -28.28302905045270421, 36.20688177001763819, -148.1802150528449999 ) ) ;
#20754 = SHAPE_REPRESENTATION_RELATIONSHIP ( 'NONE' , 'NONE' ,  #6152, #8081 ) ;
#20755 = ORIENTED_EDGE ( 'NONE', *, *, #2855, .F. ) ;
#20756 = VECTOR ( 'NONE', #11864, 1000.000000000000000 ) ;
#20757 = DIRECTION ( 'NONE',  ( 5.094701932209999624E-24, 1.000000000000000000, 0.000000000000000000 ) ) ;
#20758 = DIRECTION ( 'NONE',  ( -2.507771768019999718E-12, -1.592654864069999939E-17, 1.000000000000000000 ) ) ;
#20759 = VECTOR ( 'NONE', #22889, 1000.000000000000000 ) ;
#20760 = FACE_OUTER_BOUND ( 'NONE', #2779, .T. ) ;
#20761 = ORIENTED_EDGE ( 'NONE', *, *, #2669, .T. ) ;
#20762 = CARTESIAN_POINT ( 'NONE',  ( 6.500000000040000003, 20.50000000000000000, -136.0552959530000123 ) ) ;
#20763 = CARTESIAN_POINT ( 'NONE',  ( -25.86630785139999844, -51.50000000000000000, -137.0552959530000123 ) ) ;
#20764 = ORIENTED_EDGE ( 'NONE', *, *, #10136, .T. ) ;
#20765 = CARTESIAN_POINT ( 'NONE',  ( -21.90852802850000103, 37.90475843469999973, -148.1502781210000137 ) ) ;
#20766 = CARTESIAN_POINT ( 'NONE',  ( -18.94796313193197079, 38.67526590167940981, -147.5829755502408318 ) ) ;
#20767 = CARTESIAN_POINT ( 'NONE',  ( 7.940121941277687334, 38.39185605419793035, -146.1320387297646448 ) ) ;
#20768 = CARTESIAN_POINT ( 'NONE',  ( -32.50000000000000000, 47.50000000000000000, -137.0552959530000123 ) ) ;
#20769 = ADVANCED_FACE ( 'NONE', ( #14170 ), #6902, .F. ) ;
#20770 = CARTESIAN_POINT ( 'NONE',  ( -25.47266295436726580, 33.45219305391066200, -144.4863246959951084 ) ) ;
#20771 = LINE ( 'NONE', #22667, #13938 ) ;
#20772 = ORIENTED_EDGE ( 'NONE', *, *, #17365, .T. ) ;
#20773 = DIRECTION ( 'NONE',  ( 0.9848077530125619594, 0.000000000000000000, 0.1736481776649230202 ) ) ;
#20774 = ORIENTED_EDGE ( 'NONE', *, *, #393, .T. ) ;
#20775 = CARTESIAN_POINT ( 'NONE',  ( 16.13369214859999801, -50.50000000000000000, -136.0552959530000123 ) ) ;
#20776 = ORIENTED_EDGE ( 'NONE', *, *, #6768, .T. ) ;
#20777 =( LENGTH_UNIT ( ) NAMED_UNIT ( * ) SI_UNIT ( .MILLI., .METRE. ) );
#20778 = ORIENTED_EDGE ( 'NONE', *, *, #12190, .T. ) ;
#20779 = DIRECTION ( 'NONE',  ( 2.255973186040000320E-12, 0.000000000000000000, 1.000000000000000000 ) ) ;
#20780 = ORIENTED_EDGE ( 'NONE', *, *, #16266, .F. ) ;
#20781 = CARTESIAN_POINT ( 'NONE',  ( -0.9519686233182992341, 21.48063989304531063, -136.0552959529978523 ) ) ;
#20782 = ORIENTED_EDGE ( 'NONE', *, *, #7034, .F. ) ;
#20783 = VECTOR ( 'NONE', #11471, 1000.000000000000000 ) ;
#20784 = ORIENTED_EDGE ( 'NONE', *, *, #18623, .F. ) ;
#20785 = CARTESIAN_POINT ( 'NONE',  ( -4.521812268179999705, -27.38504028299999860, -147.5552959529999839 ) ) ;
#20786 = CARTESIAN_POINT ( 'NONE',  ( 13.13369214859999978, 50.50000000000000000, -137.0552959530000123 ) ) ;
#20787 = VECTOR ( 'NONE', #3450, 1000.000000000000000 ) ;
#20788 = CARTESIAN_POINT ( 'NONE',  ( -11.21635108262976388, 37.71473148017482657, -140.6865916277538133 ) ) ;
#20789 = CARTESIAN_POINT ( 'NONE',  ( -30.49999999990000177, 26.50000000000000000, -139.0552959529999839 ) ) ;
#20790 = CARTESIAN_POINT ( 'NONE',  ( -6.565507373411109349, 37.00519331013509827, -148.7410818962521830 ) ) ;
#20791 = CARTESIAN_POINT ( 'NONE',  ( -9.460728761480464044, 37.99149710710148042, -148.7262519339525966 ) ) ;
#20792 = ORIENTED_EDGE ( 'NONE', *, *, #5158, .T. ) ;
#20793 = CARTESIAN_POINT ( 'NONE',  ( 13.13369214859999978, -51.00000000000000000, -137.0552959530000123 ) ) ;
#20794 = EDGE_CURVE ( 'NONE', #915, #21589, #8669, .T. ) ;
#20795 = CARTESIAN_POINT ( 'NONE',  ( 9.861913442962562115, 36.36936048521160103, -146.4749235844630846 ) ) ;
#20796 = CARTESIAN_POINT ( 'NONE',  ( 24.01497134762854913, 33.88109793996614627, -150.0552959529999839 ) ) ;
#20797 = EDGE_CURVE ( 'NONE', #22055, #4267, #5118, .T. ) ;
#20798 = ORIENTED_EDGE ( 'NONE', *, *, #9407, .F. ) ;
#20799 = VECTOR ( 'NONE', #10062, 1000.000000000000227 ) ;
#20800 = FACE_OUTER_BOUND ( 'NONE', #22319, .T. ) ;
#20801 = DIRECTION ( 'NONE',  ( 1.000000000000000000, 0.000000000000000000, -2.275957200481568888E-12 ) ) ;
#20802 = VECTOR ( 'NONE', #8356, 1000.000000000000000 ) ;
#20803 = ORIENTED_EDGE ( 'NONE', *, *, #13478, .T. ) ;
#20804 =( NAMED_UNIT ( * ) SI_UNIT ( $, .STERADIAN. ) SOLID_ANGLE_UNIT ( ) );
#20805 = FACE_OUTER_BOUND ( 'NONE', #8931, .T. ) ;
#20806 = EDGE_LOOP ( 'NONE', ( #18601, #4858, #12717, #14368 ) ) ;
#20807 = CARTESIAN_POINT ( 'NONE',  ( 22.50000000000000000, 39.50000000000000000, -136.5552959530000123 ) ) ;
#20808 = DIRECTION ( 'NONE',  ( 0.000000000000000000, 6.264364525598899972E-11, -1.000000000000000000 ) ) ;
#20809 = EDGE_LOOP ( 'NONE', ( #2116, #19507, #14140, #18510 ) ) ;
#20810 = CARTESIAN_POINT ( 'NONE',  ( -14.78687493254208363, 41.11828399665055400, -141.6185954194986039 ) ) ;
#20811 = CARTESIAN_POINT ( 'NONE',  ( -25.33725402850548036, 34.39035690846336024, -140.4300890444341974 ) ) ;
#20812 = ORIENTED_EDGE ( 'NONE', *, *, #7785, .T. ) ;
#20813 = EDGE_CURVE ( 'NONE', #18344, #12998, #7177, .T. ) ;
#20814 = LINE ( 'NONE', #10075, #910 ) ;
#20815 = ORIENTED_EDGE ( 'NONE', *, *, #1490, .T. ) ;
#20816 = FACE_OUTER_BOUND ( 'NONE', #6217, .T. ) ;
#20817 = DIRECTION ( 'NONE',  ( 8.955190032049010580E-12, -9.104778821567928717E-13, 1.000000000000000000 ) ) ;
#20818 = EDGE_LOOP ( 'NONE', ( #10040, #13131, #9416, #18367 ) ) ;
#20819 = CARTESIAN_POINT ( 'NONE',  ( -21.35824191589999899, -31.25000000000000000, -146.3157682190075093 ) ) ;
#20820 = VERTEX_POINT ( 'NONE', #16308 ) ;
#20821 = CARTESIAN_POINT ( 'NONE',  ( -35.07300000000000040, 11.44852983560000048, -143.5552959529999839 ) ) ;
#20822 = VECTOR ( 'NONE', #9260, 1000.000000000000000 ) ;
#20823 = FACE_OUTER_BOUND ( 'NONE', #5974, .T. ) ;
#20824 = ORIENTED_EDGE ( 'NONE', *, *, #10598, .T. ) ;
#20825 = EDGE_CURVE ( 'NONE', #3203, #4135, #14770, .T. ) ;
#20826 = EDGE_CURVE ( 'NONE', #21589, #22524, #19717, .T. ) ;
#20827 = ORIENTED_EDGE ( 'NONE', *, *, #11999, .T. ) ;
#20828 = DIRECTION ( 'NONE',  ( -1.000000000000000000, 0.000000000000000000, 0.000000000000000000 ) ) ;
#20829 = CARTESIAN_POINT ( 'NONE',  ( -31.50000000000000000, 14.00000000000000000, -144.0552959529999839 ) ) ;
#20830 = CARTESIAN_POINT ( 'NONE',  ( -26.47299999999999898, 12.24483487620000055, -145.0141470300000037 ) ) ;
#20831 = DIRECTION ( 'NONE',  ( 1.526468026909999897E-13, 8.159623473500000156E-13, 1.000000000000000000 ) ) ;
#20832 = ORIENTED_EDGE ( 'NONE', *, *, #10591, .F. ) ;
#20833 = CARTESIAN_POINT ( 'NONE',  ( -7.499999999969999109, 48.50000000000000000, -137.0552959530000123 ) ) ;
#20834 = CARTESIAN_POINT ( 'NONE',  ( -7.828824709450000086, 39.51093879980000168, -140.6700787229999889 ) ) ;
#20835 = AXIS2_PLACEMENT_3D ( 'NONE', #14294, #21565, #21688 ) ;
#20836 = LINE ( 'NONE', #4532, #4488 ) ;
#20837 = DIRECTION ( 'NONE',  ( -0.1778629393740580045, -0.9840552701943220404, 3.562475540061165072E-13 ) ) ;
#20838 = LINE ( 'NONE', #6664, #20855 ) ;
#20839 = VECTOR ( 'NONE', #7905, 999.9999999999998863 ) ;
#20840 = VERTEX_POINT ( 'NONE', #9022 ) ;
#20841 = CARTESIAN_POINT ( 'NONE',  ( -16.36060017231690011, 36.32623467514464721, -140.3335547247180841 ) ) ;
#20842 = CARTESIAN_POINT ( 'NONE',  ( -16.15870017774198431, 34.84090251771772273, -146.9067376896876453 ) ) ;
#20843 = CARTESIAN_POINT ( 'NONE',  ( -5.558768696239984486, 37.82651365785675779, -139.8085169320104058 ) ) ;
#20844 = DIRECTION ( 'NONE',  ( 0.000000000000000000, -1.000000000000000000, 0.000000000000000000 ) ) ;
#20845 = CARTESIAN_POINT ( 'NONE',  ( 24.38136133040000075, -29.22855050349999928, -146.5552959529999839 ) ) ;
#20846 = EDGE_CURVE ( 'NONE', #6638, #11714, #8793, .T. ) ;
#20847 = ORIENTED_EDGE ( 'NONE', *, *, #15642, .F. ) ;
#20848 =( BOUNDED_CURVE ( )  B_SPLINE_CURVE ( 5, ( #16993, #2606, #4276, #6396, #13657, #16881 ),
 .UNSPECIFIED., .F., .F. ) 
 B_SPLINE_CURVE_WITH_KNOTS ( ( 6, 6 ),
 ( 1.570796326702242673, 3.141592653590000062 ),
 .UNSPECIFIED. ) 
 CURVE ( )  GEOMETRIC_REPRESENTATION_ITEM ( )  RATIONAL_B_SPLINE_CURVE ( ( 0.2500000000000000000, 0.2499999999881897805, 0.2999999999822846597, 0.3999999999763795278, 0.5999999999763795389, 1.000000000000000000 ) ) 
 REPRESENTATION_ITEM ( '' )  );
#20849 = CARTESIAN_POINT ( 'NONE',  ( -9.072898850179999641, 36.94639249900000522, -148.2684494029999769 ) ) ;
#20850 = DIRECTION ( 'NONE',  ( -2.257144641399999941E-12, 8.049635416090000264E-35, -1.000000000000000000 ) ) ;
#20851 = CARTESIAN_POINT ( 'NONE',  ( 23.50000000000000000, -20.50000000000000000, -144.7152959530000089 ) ) ;
#20852 = VERTEX_POINT ( 'NONE', #3579 ) ;
#20853 = CARTESIAN_POINT ( 'NONE',  ( 11.68320006079999906, -20.50000000000000000, -148.5552959529999839 ) ) ;
#20854 = VECTOR ( 'NONE', #7467, 1000.000000000000000 ) ;
#20855 = VECTOR ( 'NONE', #17733, 1000.000000000000000 ) ;
#20856 = CARTESIAN_POINT ( 'NONE',  ( -28.37825339583908146, 32.94869610820727246, -141.6352474658712026 ) ) ;
#20857 = ADVANCED_FACE ( 'NONE', ( #7020 ), #21905, .T. ) ;
#20858 = DIRECTION ( 'NONE',  ( 0.000000000000000000, -1.000000000000000000, 8.159623473500000156E-13 ) ) ;
#20859 = EDGE_LOOP ( 'NONE', ( #3701, #12611, #10430, #14966 ) ) ;
#20860 = AXIS2_PLACEMENT_3D ( 'NONE', #6144, #2361, #7913 ) ;
#20861 = CARTESIAN_POINT ( 'NONE',  ( -23.24386692375823316, 40.83902259678306024, -144.5872313496660695 ) ) ;
#20862 = DIRECTION ( 'NONE',  ( 1.000000000000000000, 0.000000000000000000, 2.516505522483685870E-12 ) ) ;
#20863 = AXIS2_PLACEMENT_3D ( 'NONE', #22143, #494, #5829 ) ;
#20864 = CARTESIAN_POINT ( 'NONE',  ( -15.57786843150000067, 37.00666880280000726, -148.5521201120000114 ) ) ;
#20865 = DIRECTION ( 'NONE',  ( 2.257242012349999735E-12, 0.000000000000000000, -1.000000000000000000 ) ) ;
#20866 = FACE_BOUND ( 'NONE', #1945, .T. ) ;
#20867 = DIRECTION ( 'NONE',  ( -0.9892101392001054760, 0.1465035852930155480, 4.471739159800472250E-12 ) ) ;
#20868 = CARTESIAN_POINT ( 'NONE',  ( -8.561883997267385027, 37.68227764167581029, -140.5058735119322648 ) ) ;
#20869 = EDGE_CURVE ( 'NONE', #17719, #18084, #21551, .T. ) ;
#20870 = ORIENTED_EDGE ( 'NONE', *, *, #98, .F. ) ;
#20871 = PRESENTATION_STYLE_ASSIGNMENT (( #13847 ) ) ;
#20872 = VECTOR ( 'NONE', #13805, 1000.000000000000000 ) ;
#20873 = VECTOR ( 'NONE', #8355, 1000.000000000000000 ) ;
#20874 = VERTEX_POINT ( 'NONE', #17978 ) ;
#20875 = CARTESIAN_POINT ( 'NONE',  ( -14.60018857135958292, 36.05920633199687586, -140.1047136458358864 ) ) ;
#20876 = LINE ( 'NONE', #6235, #17564 ) ;
#20877 = CARTESIAN_POINT ( 'NONE',  ( -2.499999999839999987, 41.50000000000000000, -140.5552959529999839 ) ) ;
#20878 = VECTOR ( 'NONE', #6669, 1000.000000000000000 ) ;
#20879 = ADVANCED_FACE ( 'NONE', ( #7263 ), #1688, .F. ) ;
#20880 = VERTEX_POINT ( 'NONE', #7943 ) ;
#20881 = AXIS2_PLACEMENT_3D ( 'NONE', #20982, #4673, #21781 ) ;
#20882 = CARTESIAN_POINT ( 'NONE',  ( -25.85824191589999899, -34.50000000000000000, -146.3157682190000060 ) ) ;
#20883 = CARTESIAN_POINT ( 'NONE',  ( -6.635402838459999231, -21.69968975860000171, -146.5552959529999839 ) ) ;
#20884 = ADVANCED_FACE ( 'NONE', ( #11509 ), #481, .T. ) ;
#20885 = ORIENTED_EDGE ( 'NONE', *, *, #9511, .T. ) ;
#20886 = FACE_OUTER_BOUND ( 'NONE', #14952, .T. ) ;
#20887 = EDGE_CURVE ( 'NONE', #11360, #19834, #11396, .T. ) ;
#20888 = ADVANCED_FACE ( 'NONE', ( #16766 ), #14983, .T. ) ;
#20889 = CARTESIAN_POINT ( 'NONE',  ( -17.72712734282866265, 38.71922357431461847, -139.9447469178576000 ) ) ;
#20890 = CARTESIAN_POINT ( 'NONE',  ( 8.037076569876626664, 38.42714480829248913, -146.1079377423441201 ) ) ;
#20891 = AXIS2_PLACEMENT_3D ( 'NONE', #1591, #15969, #19302 ) ;
#20892 = CARTESIAN_POINT ( 'NONE',  ( 20.50000000000000000, 22.50000000000000000, -150.0552959529999839 ) ) ;
#20893 = APPLICATION_CONTEXT ( 'automotive_design' ) ;
#20894 = VECTOR ( 'NONE', #1681, 1000.000000000000227 ) ;
#20895 = CARTESIAN_POINT ( 'NONE',  ( -25.08423778095658463, 34.60282621925794189, -140.6697649010042426 ) ) ;
#20896 = CARTESIAN_POINT ( 'NONE',  ( 4.698575659218127143, -5.000067229902920296, -150.0552959529999839 ) ) ;
#20897 = VECTOR ( 'NONE', #687, 1000.000000000000000 ) ;
#20898 =( BOUNDED_CURVE ( )  B_SPLINE_CURVE ( 5, ( #22039, #5498, #16330, #7504, #18456, #3712, #5838, #14655, #10827, #2060, #13094, #16668 ),
 .UNSPECIFIED., .F., .F. ) 
 B_SPLINE_CURVE_WITH_KNOTS ( ( 6, 3, 3, 6 ),
 ( 0.000000000000000000, 4.463483057499999518, 8.880954762089999122, 13.25426345570000031 ),
 .UNSPECIFIED. ) 
 CURVE ( )  GEOMETRIC_REPRESENTATION_ITEM ( )  RATIONAL_B_SPLINE_CURVE ( ( 0.2500000000000000000, 0.2500000000000000000, 0.2500000000000000000, 0.2500000000000000000, 0.2500000000000000000, 0.2500000000000000000, 0.2500000000000000000, 0.2500000000000000000, 0.2500000000000000000, 0.2500000000000000000, 0.2500000000000000000, 0.2500000000000000000 ) ) 
 REPRESENTATION_ITEM ( '' )  );
#20899 = VECTOR ( 'NONE', #18649, 1000.000000000000000 ) ;
#20900 = VECTOR ( 'NONE', #11621, 1000.000000000000227 ) ;
#20901 = ORIENTED_EDGE ( 'NONE', *, *, #9804, .T. ) ;
#20902 = FACE_OUTER_BOUND ( 'NONE', #5088, .T. ) ;
#20903 = VERTEX_POINT ( 'NONE', #3930 ) ;
#20904 =( NAMED_UNIT ( * ) SI_UNIT ( $, .STERADIAN. ) SOLID_ANGLE_UNIT ( ) );
#20905 = EDGE_LOOP ( 'NONE', ( #2363, #20026, #7635, #22720 ) ) ;
#20906 = DIRECTION ( 'NONE',  ( 0.000000000000000000, 1.000000000000000000, 2.245315043809999812E-12 ) ) ;
#20907 = EDGE_LOOP ( 'NONE', ( #16337, #14380, #3756, #19559 ) ) ;
#20908 = CARTESIAN_POINT ( 'NONE',  ( -30.49999999990000177, 34.50000000000000000, -144.0552959529999839 ) ) ;
#20909 = ORIENTED_EDGE ( 'NONE', *, *, #3703, .T. ) ;
#20910 = ORIENTED_EDGE ( 'NONE', *, *, #18884, .F. ) ;
#20911 = CARTESIAN_POINT ( 'NONE',  ( -32.50000000000000000, 1.000000000000000000, -149.5552959529999839 ) ) ;
#20912 = CARTESIAN_POINT ( 'NONE',  ( -9.971101149720000834, 37.05360750090000721, -147.8421425029999909 ) ) ;
#20913 = ADVANCED_FACE ( 'NONE', ( #9610 ), #4041, .F. ) ;
#20914 = PLANE ( 'NONE',  #19101 ) ;
#20915 = LINE ( 'NONE', #15676, #18189 ) ;
#20916 = AXIS2_PLACEMENT_3D ( 'NONE', #9786, #15048, #11691 ) ;
#20917 = CIRCLE ( 'NONE', #17872, 0.5000000000000004441 ) ;
#20918 = CARTESIAN_POINT ( 'NONE',  ( -7.712174556309761009, 32.67941313690337068, -141.7048212837721621 ) ) ;
#20919 = AXIS2_PLACEMENT_3D ( 'NONE', #8884, #10901, #7349 ) ;
#20920 = LINE ( 'NONE', #4608, #3392 ) ;
#20921 = VERTEX_POINT ( 'NONE', #16536 ) ;
#20922 = PLANE ( 'NONE',  #8297 ) ;
#20923 = CARTESIAN_POINT ( 'NONE',  ( 9.253750895402886201, 35.69920382850602891, -146.1911047861467807 ) ) ;
#20924 = LINE ( 'NONE', #15325, #14034 ) ;
#20925 = ORIENTED_EDGE ( 'NONE', *, *, #15327, .T. ) ;
#20926 = DIRECTION ( 'NONE',  ( -1.000000000000000000, 0.000000000000000000, 0.000000000000000000 ) ) ;
#20927 = DIRECTION ( 'NONE',  ( 1.000000000000000000, 0.000000000000000000, 0.000000000000000000 ) ) ;
#20928 = ORIENTED_EDGE ( 'NONE', *, *, #1401, .T. ) ;
#20929 = LINE ( 'NONE', #5087, #20756 ) ;
#20930 = VECTOR ( 'NONE', #488, 1000.000000000000000 ) ;
#20931 = AXIS2_PLACEMENT_3D ( 'NONE', #1646, #14479, #19948 ) ;
#20932 = VERTEX_POINT ( 'NONE', #15227 ) ;
#20933 = FACE_BOUND ( 'NONE', #13333, .T. ) ;
#20934 = DIRECTION ( 'NONE',  ( 0.000000000000000000, 0.000000000000000000, 1.000000000000000000 ) ) ;
#20935 = VERTEX_POINT ( 'NONE', #13189 ) ;
#20936 = CARTESIAN_POINT ( 'NONE',  ( -14.45293675682532886, 38.87179601339980906, -139.7374547563314593 ) ) ;
#20937 = CARTESIAN_POINT ( 'NONE',  ( -26.10314130450000292, 34.70878586860000325, -141.0128996759999893 ) ) ;
#20938 = VERTEX_POINT ( 'NONE', #11165 ) ;
#20939 = SURFACE_STYLE_FILL_AREA ( #17600 ) ;
#20940 = CARTESIAN_POINT ( 'NONE',  ( -2.499999999959999997, -2.273736754430000208E-12, -136.0552959530000123 ) ) ;
#20941 = ADVANCED_FACE ( 'NONE', ( #6172 ), #18438, .F. ) ;
#20942 = ORIENTED_EDGE ( 'NONE', *, *, #15058, .F. ) ;
#20943 = DIRECTION ( 'NONE',  ( -1.000000000000000000, 0.000000000000000000, 2.257453483404484831E-12 ) ) ;
#20944 = CARTESIAN_POINT ( 'NONE',  ( -8.916553640509999212, -11.88594259849999979, -143.5552959529999839 ) ) ;
#20945 = EDGE_CURVE ( 'NONE', #15811, #6002, #11556, .T. ) ;
#20946 = ORIENTED_EDGE ( 'NONE', *, *, #15760, .T. ) ;
#20947 = PLANE ( 'NONE',  #4946 ) ;
#20948 = ORIENTED_EDGE ( 'NONE', *, *, #15196, .F. ) ;
#20949 = CARTESIAN_POINT ( 'NONE',  ( 2.500000000150000012, 16.50000000000000000, -143.5552959529999839 ) ) ;
#20950 = CARTESIAN_POINT ( 'NONE',  ( -1.753667363927367884, 45.51009696919515335, -136.0552959529960617 ) ) ;
#20951 = ORIENTED_EDGE ( 'NONE', *, *, #7070, .T. ) ;
#20952 = CIRCLE ( 'NONE', #14859, 0.7500000000000006661 ) ;
#20953 =( GEOMETRIC_REPRESENTATION_CONTEXT ( 3 ) GLOBAL_UNCERTAINTY_ASSIGNED_CONTEXT ( ( #10868 ) ) GLOBAL_UNIT_ASSIGNED_CONTEXT ( ( #13599, #3250, #2790 ) ) REPRESENTATION_CONTEXT ( 'NONE', 'WORKASPACE' ) );
#20954 = ORIENTED_EDGE ( 'NONE', *, *, #3107, .F. ) ;
#20955 = CARTESIAN_POINT ( 'NONE',  ( 1.584389485034097822, -18.56644239314076117, -143.5552959530000692 ) ) ;
#20956 = DIRECTION ( 'NONE',  ( 2.257157423930000049E-12, 0.000000000000000000, 1.000000000000000000 ) ) ;
#20957 = FACE_OUTER_BOUND ( 'NONE', #22558, .T. ) ;
#20958 = PLANE ( 'NONE',  #16700 ) ;
#20959 = PRODUCT_DEFINITION_SHAPE ( 'NONE', 'NONE',  #23551 ) ;
#20960 = ORIENTED_EDGE ( 'NONE', *, *, #14487, .F. ) ;
#20961 = CARTESIAN_POINT ( 'NONE',  ( -15.75752630172931923, -41.69025052297610756, -136.0552959529644284 ) ) ;
#20962 = DIRECTION ( 'NONE',  ( 2.506794771760000178E-12, 0.000000000000000000, -1.000000000000000000 ) ) ;
#20963 = CARTESIAN_POINT ( 'NONE',  ( 23.89269908169871925, -17.50000000000000000, -150.0552959529999839 ) ) ;
#20964 = DIRECTION ( 'NONE',  ( 2.688820921349999492E-17, -1.000000000000000000, -6.069065783950000909E-29 ) ) ;
#20965 = LINE ( 'NONE', #15251, #22490 ) ;
#20966 = LINE ( 'NONE', #4658, #22751 ) ;
#20967 = VECTOR ( 'NONE', #3112, 1000.000000000000000 ) ;
#20968 = ORIENTED_EDGE ( 'NONE', *, *, #17106, .T. ) ;
#20969 = PRESENTATION_LAYER_ASSIGNMENT (  '', '', ( #22097 ) ) ;
#20970 = PLANE ( 'NONE',  #19439 ) ;
#20971 = EDGE_CURVE ( 'NONE', #7451, #11927, #4157, .T. ) ;
#20972 = DIRECTION ( 'NONE',  ( -1.000000000000000000, 1.734728570689999873E-18, 2.257171095940000041E-12 ) ) ;
#20973 = CARTESIAN_POINT ( 'NONE',  ( -4.527137292580695416, 37.91261575257937722, -140.0120598367263085 ) ) ;
#20974 = CYLINDRICAL_SURFACE ( 'NONE', #2744, 7.000000000000000888 ) ;
#20975 = EDGE_CURVE ( 'NONE', #1657, #4706, #593, .T. ) ;
#20976 = LINE ( 'NONE', #20845, #5863 ) ;
#20977 = ORIENTED_EDGE ( 'NONE', *, *, #18827, .T. ) ;
#20978 = CARTESIAN_POINT ( 'NONE',  ( -9.238580206868249434, 35.38369298950671293, -147.3609278768369677 ) ) ;
#20979 = CARTESIAN_POINT ( 'NONE',  ( 1.133692148650000009, 51.50000000000000000, -136.0552959530000123 ) ) ;
#20980 = CARTESIAN_POINT ( 'NONE',  ( -6.635402838469999232, -21.69968975860000171, -147.0552959529999839 ) ) ;
#20981 = EDGE_LOOP ( 'NONE', ( #8648, #14836, #17796, #8138 ) ) ;
#20982 = CARTESIAN_POINT ( 'NONE',  ( 4.500000000009999113, -3.500000000000000000, -136.0552959530000123 ) ) ;
#20983 = PRESENTATION_LAYER_ASSIGNMENT (  '', '', ( #19841 ) ) ;
#20984 = CARTESIAN_POINT ( 'NONE',  ( 32.50000000000000000, -33.03620104880000241, -131.8162870490000103 ) ) ;
#20985 = VERTEX_POINT ( 'NONE', #5706 ) ;
#20986 = CIRCLE ( 'NONE', #464, 2.999999999999999112 ) ;
#20987 = CARTESIAN_POINT ( 'NONE',  ( -22.79386933270184556, 37.02723109250518263, -140.7029355817512339 ) ) ;
#20988 = LINE ( 'NONE', #4678, #8950 ) ;
#20989 = CARTESIAN_POINT ( 'NONE',  ( -0.9520167400862425966, 19.51924065639807537, -150.0552959530000123 ) ) ;
#20990 = CARTESIAN_POINT ( 'NONE',  ( 9.152949117189999484, -16.59780702190000312, -148.0552959529999839 ) ) ;
#20991 = CARTESIAN_POINT ( 'NONE',  ( -10.38572958583939254, 32.19234684762017196, -144.3174661366601299 ) ) ;
#20992 = CARTESIAN_POINT ( 'NONE',  ( 1.364575185789999923, -21.31553777220000256, -143.5552959529999839 ) ) ;
#20993 = CARTESIAN_POINT ( 'NONE',  ( -7.149448239889999890, -25.45628515800000002, -145.5552959529999839 ) ) ;
#20994 = ORIENTED_EDGE ( 'NONE', *, *, #18735, .F. ) ;
#20995 = ORIENTED_EDGE ( 'NONE', *, *, #20371, .T. ) ;
#20996 = CARTESIAN_POINT ( 'NONE',  ( -7.081915218507915277, 37.06683495603981271, -147.7519347215450409 ) ) ;
#20997 = CARTESIAN_POINT ( 'NONE',  ( -26.39256767719999885, 41.50003988699999979, -143.5805134120000162 ) ) ;
#20998 = COLOUR_RGB ( '', 0.66274510, 0.83137255, 0.94901961) ;
#20999 = DIRECTION ( 'NONE',  ( 2.257749542879999954E-12, 0.000000000000000000, 1.000000000000000000 ) ) ;
#21000 = AXIS2_PLACEMENT_3D ( 'NONE', #20587, #4050, #491 ) ;
#21001 = ORIENTED_EDGE ( 'NONE', *, *, #5153, .T. ) ;
#21002 = PLANE ( 'NONE',  #5338 ) ;
#21003 = CARTESIAN_POINT ( 'NONE',  ( 0.1832000607640000001, -6.500000000000000000, -148.5552959529999839 ) ) ;
#21004 = ORIENTED_EDGE ( 'NONE', *, *, #21566, .F. ) ;
#21005 = CARTESIAN_POINT ( 'NONE',  ( -21.31094475132173471, 38.36490538190786737, -147.1930922076768411 ) ) ;
#21006 = EDGE_CURVE ( 'NONE', #10871, #3534, #20690, .T. ) ;
#21007 = CARTESIAN_POINT ( 'NONE',  ( -17.01025018536428135, 38.48180121065468029, -140.7067500820375869 ) ) ;
#21008 = CARTESIAN_POINT ( 'NONE',  ( -16.84364015992474606, -40.60099947280546218, -150.0552959529999839 ) ) ;
#21009 = CARTESIAN_POINT ( 'NONE',  ( 7.587328409695290432, 38.19466532143988502, -146.2522312777784634 ) ) ;
#21010 = LINE ( 'NONE', #11347, #9316 ) ;
#21011 = CARTESIAN_POINT ( 'NONE',  ( -24.69700618074178777, 35.61223127418029577, -147.2014722472205506 ) ) ;
#21012 = DIRECTION ( 'NONE',  ( 5.094701932209999624E-24, 1.000000000000000000, 0.000000000000000000 ) ) ;
#21013 = CARTESIAN_POINT ( 'NONE',  ( -12.35737375542222161, 41.41429090104503530, -143.6540282846627576 ) ) ;
#21014 = AXIS2_PLACEMENT_3D ( 'NONE', #19176, #15729, #23225 ) ;
#21015 = ADVANCED_FACE ( 'NONE', ( #18548 ), #2152, .T. ) ;
#21016 = EDGE_CURVE ( 'NONE', #23105, #18841, #358, .T. ) ;
#21017 = EDGE_LOOP ( 'NONE', ( #6631, #16250, #19178, #17083 ) ) ;
#21018 = DIRECTION ( 'NONE',  ( 2.257171095940000041E-12, 1.003664318210000046E-28, 1.000000000000000000 ) ) ;
#21019 = EDGE_CURVE ( 'NONE', #22307, #4100, #3375, .T. ) ;
#21020 = EDGE_LOOP ( 'NONE', ( #22058, #8225, #9960 ) ) ;
#21021 = ORIENTED_EDGE ( 'NONE', *, *, #3959, .F. ) ;
#21022 = CARTESIAN_POINT ( 'NONE',  ( 4.999999999879999990, -3.000000000000000000, -135.4552959529999896 ) ) ;
#21023 = EDGE_CURVE ( 'NONE', #17988, #22710, #16667, .T. ) ;
#21024 = VERTEX_POINT ( 'NONE', #14015 ) ;
#21025 = DIRECTION ( 'NONE',  ( 2.257157423930000049E-12, 0.000000000000000000, 1.000000000000000000 ) ) ;
#21026 = ORIENTED_EDGE ( 'NONE', *, *, #21182, .T. ) ;
#21027 = ORIENTED_EDGE ( 'NONE', *, *, #2558, .T. ) ;
#21028 = PRODUCT ( 'Spindle Hub', 'Spindle Hub', '', ( #16402 ) ) ;
#21029 = CARTESIAN_POINT ( 'NONE',  ( 2.500000000130000011, 24.50000000000000000, -150.5552959529999839 ) ) ;
#21030 = CARTESIAN_POINT ( 'NONE',  ( -19.33778615812330415, 35.56580707893081694, -147.6585156976900919 ) ) ;
#21031 = CARTESIAN_POINT ( 'NONE',  ( -11.48759298139373897, 37.74537190003064069, -140.3874188149447946 ) ) ;
#21032 = PRODUCT_DEFINITION_FORMATION_WITH_SPECIFIED_SOURCE ( 'ANY', '', #11988, .NOT_KNOWN. ) ;
#21033 = CARTESIAN_POINT ( 'NONE',  ( -7.254103886545301805, 34.31303075260233726, -140.3989650697497495 ) ) ;
#21034 = LINE ( 'NONE', #13882, #7200 ) ;
#21035 = ORIENTED_EDGE ( 'NONE', *, *, #11810, .T. ) ;
#21036 = EDGE_CURVE ( 'NONE', #4093, #5749, #6283, .T. ) ;
#21037 = CARTESIAN_POINT ( 'NONE',  ( 7.750000000030000002, -2.273736754430000208E-12, -136.0552959530000123 ) ) ;
#21038 =( BOUNDED_SURFACE ( )  B_SPLINE_SURFACE ( 5, 5, ( 
 ( #4160, #5820, #18900, #2610, #22017, #9841 ),
 ( #11510, #360, #16885, #20238, #20579, #9721 ),
 ( #17120, #7484, #13077, #14748, #11167, #16646 ),
 ( #13424, #16997, #7718, #18439, #4386, #7946 ),
 ( #482, #14984, #5707, #12961, #594, #3931 ),
 ( #4043, #2154, #9373, #15228, #7601, #20463 ),
 ( #22480, #18789, #14875, #22133, #6173, #2500 ),
 ( #11277, #7829, #20349, #18550, #2270, #9495 ),
 ( #16767, #22244, #5937, #13190, #18678, #11397 ),
 ( #2390, #9611, #15100, #22360, #6059, #13311 ),
 ( #4280, #711, #20691, #19558, #13957, #2903 ),
 ( #22897, #10017, #14084, #12047, #17410, #6582 ) ),
 .UNSPECIFIED., .F., .F., .F. ) 
 B_SPLINE_SURFACE_WITH_KNOTS ( ( 6, 3, 3, 6 ),
 ( 6, 6 ),
 ( 0.000000000000000000, 4.390059406679999832, 8.746277600790000051, 13.07048654049999925 ),
 ( 0.000000000000000000, 1.570796326702240009 ),
 .UNSPECIFIED. ) 
 GEOMETRIC_REPRESENTATION_ITEM ( )  RATIONAL_B_SPLINE_SURFACE ( (
 ( 1.000000000000000000, 0.6000000000236209718, 0.4000000000236205167, 0.3000000000177154846, 0.2500000000118104970, 0.2500000000000000000),
 ( 1.000000000000000000, 0.6000000000236209718, 0.4000000000236205167, 0.3000000000177154846, 0.2500000000118104970, 0.2500000000000000000),
 ( 1.000000000000000000, 0.6000000000236209718, 0.4000000000236205167, 0.3000000000177154846, 0.2500000000118104970, 0.2500000000000000000),
 ( 1.000000000000000000, 0.6000000000236209718, 0.4000000000236205167, 0.3000000000177154846, 0.2500000000118104970, 0.2500000000000000000),
 ( 1.000000000000000000, 0.6000000000236209718, 0.4000000000236205167, 0.3000000000177154846, 0.2500000000118104970, 0.2500000000000000000),
 ( 1.000000000000000000, 0.6000000000236209718, 0.4000000000236205167, 0.3000000000177154846, 0.2500000000118104970, 0.2500000000000000000),
 ( 1.000000000000000000, 0.6000000000236209718, 0.4000000000236205167, 0.3000000000177154846, 0.2500000000118104970, 0.2500000000000000000),
 ( 1.000000000000000000, 0.6000000000236209718, 0.4000000000236205167, 0.3000000000177154846, 0.2500000000118104970, 0.2500000000000000000),
 ( 1.000000000000000000, 0.6000000000236209718, 0.4000000000236205167, 0.3000000000177154846, 0.2500000000118104970, 0.2500000000000000000),
 ( 1.000000000000000000, 0.6000000000236209718, 0.4000000000236205167, 0.3000000000177154846, 0.2500000000118104970, 0.2500000000000000000),
 ( 1.000000000000000000, 0.6000000000236209718, 0.4000000000236205167, 0.3000000000177154846, 0.2500000000118104970, 0.2500000000000000000),
 ( 1.000000000000000000, 0.6000000000236209718, 0.4000000000236205167, 0.3000000000177154846, 0.2500000000118104970, 0.2500000000000000000) ) ) 
 REPRESENTATION_ITEM ( '' )  SURFACE ( )  );
#21039 = CARTESIAN_POINT ( 'NONE',  ( -14.58163105939557624, 36.93319896293952098, -139.6872257168654414 ) ) ;
#21040 = CARTESIAN_POINT ( 'NONE',  ( -7.499999999969999109, 19.50000000000000000, -137.0552959530000123 ) ) ;
#21041 = ORIENTED_EDGE ( 'NONE', *, *, #16824, .F. ) ;
#21042 = EDGE_CURVE ( 'NONE', #567, #5050, #837, .T. ) ;
#21043 = ADVANCED_FACE ( 'NONE', ( #19140 ), #2609, .T. ) ;
#21044 = LINE ( 'NONE', #8414, #19680 ) ;
#21045 = FACE_OUTER_BOUND ( 'NONE', #16759, .T. ) ;
#21046 = ORIENTED_EDGE ( 'NONE', *, *, #10954, .T. ) ;
#21047 = LINE ( 'NONE', #20684, #18158 ) ;
#21048 = DIRECTION ( 'NONE',  ( 0.000000000000000000, -8.980547998385300260E-15, -1.000000000000000000 ) ) ;
#21049 = ADVANCED_FACE ( 'NONE', ( #19249 ), #19516, .F. ) ;
#21050 = VERTEX_POINT ( 'NONE', #8530 ) ;
#21051 = DIRECTION ( 'NONE',  ( 2.257171095940000041E-12, 1.003664318210000046E-28, 1.000000000000000000 ) ) ;
#21052 = CARTESIAN_POINT ( 'NONE',  ( -18.75277607359999976, 37.97046254950000588, -148.4181951110000171 ) ) ;
#21053 = ORIENTED_EDGE ( 'NONE', *, *, #10355, .F. ) ;
#21054 = CARTESIAN_POINT ( 'NONE',  ( -14.23530246729999860, 39.72954597060000026, -140.2988105550000171 ) ) ;
#21055 = CARTESIAN_POINT ( 'NONE',  ( -25.17490547269999723, 35.46855981759999565, -147.6699473629999773 ) ) ;
#21056 = ORIENTED_EDGE ( 'NONE', *, *, #19287, .T. ) ;
#21057 = SURFACE_STYLE_FILL_AREA ( #15807 ) ;
#21058 = DIRECTION ( 'NONE',  ( -1.000000000000000000, 0.000000000000000000, 2.257120985840000117E-12 ) ) ;
#21059 = ORIENTED_EDGE ( 'NONE', *, *, #13454, .F. ) ;
#21060 = CARTESIAN_POINT ( 'NONE',  ( -2.499999999969999998, 34.00000000000000000, -137.0552959530000123 ) ) ;
#21061 = FACE_OUTER_BOUND ( 'NONE', #9809, .T. ) ;
#21062 = ORIENTED_EDGE ( 'NONE', *, *, #20421, .F. ) ;
#21063 = LINE ( 'NONE', #17245, #4184 ) ;
#21064 = EDGE_LOOP ( 'NONE', ( #22189, #21506, #7283, #15611, #9425 ) ) ;
#21065 = DIRECTION ( 'NONE',  ( -0.1000233216789610108, -0.9949850929136109245, 3.559993607998610461E-13 ) ) ;
#21066 = VERTEX_POINT ( 'NONE', #1309 ) ;
#21067 = FACE_OUTER_BOUND ( 'NONE', #8964, .T. ) ;
#21068 = ORIENTED_EDGE ( 'NONE', *, *, #16678, .F. ) ;
#21069 = VECTOR ( 'NONE', #11309, 1000.000000000000000 ) ;
#21070 = EDGE_LOOP ( 'NONE', ( #8256, #17416, #15932, #16302, #8629 ) ) ;
#21071 = CARTESIAN_POINT ( 'NONE',  ( -7.816799939239999162, 0.9999999999989999111, -150.0552959529999839 ) ) ;
#21072 = ADVANCED_FACE ( 'NONE', ( #15568 ), #1174, .F. ) ;
#21073 = CARTESIAN_POINT ( 'NONE',  ( 32.50000000000000000, -2.273736754430000208E-12, -136.0552959530000123 ) ) ;
#21074 = EDGE_CURVE ( 'NONE', #9406, #14014, #20115, .T. ) ;
#21075 = CARTESIAN_POINT ( 'NONE',  ( -14.12781175210000129, 38.88127384660000274, -139.8125553750000165 ) ) ;
#21076 = LINE ( 'NONE', #19275, #1527 ) ;
#21077 = ORIENTED_EDGE ( 'NONE', *, *, #4158, .F. ) ;
#21078 =( LENGTH_UNIT ( ) NAMED_UNIT ( * ) SI_UNIT ( .MILLI., .METRE. ) );
#21079 = DIRECTION ( 'NONE',  ( -0.9913873220698726785, 0.1309625047069831461, 0.000000000000000000 ) ) ;
#21080 = CARTESIAN_POINT ( 'NONE',  ( 19.50000000000000000, 51.50000000000000000, -137.0552959530000123 ) ) ;
#21081 = CARTESIAN_POINT ( 'NONE',  ( 31.64594224149999846, 40.56768785850000825, -149.5552959529999839 ) ) ;
#21082 = DIRECTION ( 'NONE',  ( -1.000000000000000000, 0.000000000000000000, 0.000000000000000000 ) ) ;
#21083 = DIRECTION ( 'NONE',  ( 2.842170943040000002E-14, 3.552713678800000097E-13, 1.000000000000000000 ) ) ;
#21084 = VERTEX_POINT ( 'NONE', #3550 ) ;
#21085 = CARTESIAN_POINT ( 'NONE',  ( -4.499999999959999109, 37.00000000000000000, -136.0552959530000123 ) ) ;
#21086 = LINE ( 'NONE', #23217, #10972 ) ;
#21087 = CARTESIAN_POINT ( 'NONE',  ( -9.394779979509999990, -17.86685386420000299, -143.5552959529999839 ) ) ;
#21088 = CARTESIAN_POINT ( 'NONE',  ( -4.428060343052311332, 37.07089632425688563, -139.9976721173915735 ) ) ;
#21089 = DIRECTION ( 'NONE',  ( 1.000000000000000000, 0.000000000000000000, 0.000000000000000000 ) ) ;
#21090 = VERTEX_POINT ( 'NONE', #23415 ) ;
#21091 = CARTESIAN_POINT ( 'NONE',  ( -9.389499115867565138, 36.98418387198957902, -147.3811924090515788 ) ) ;
#21092 = DIRECTION ( 'NONE',  ( 1.000000000000000000, 0.000000000000000000, 0.000000000000000000 ) ) ;
#21093 = CARTESIAN_POINT ( 'NONE',  ( 3.580208454387329375, -2.299235031440459931, -150.0552959529999839 ) ) ;
#21094 = EDGE_LOOP ( 'NONE', ( #6721, #21177, #3476, #1236 ) ) ;
#21095 = CARTESIAN_POINT ( 'NONE',  ( 3.249999999879999990, -4.000000000000000000, -135.4552959529999896 ) ) ;
#21096 = CARTESIAN_POINT ( 'NONE',  ( -28.52054873391283962, 32.26575815815821358, -143.5049952843087908 ) ) ;
#21097 = CARTESIAN_POINT ( 'NONE',  ( 31.00000000000000000, 39.80430157320000006, -150.5552959529999839 ) ) ;
#21098 = EDGE_LOOP ( 'NONE', ( #17251, #17650, #20946, #8244 ) ) ;
#21099 = EDGE_CURVE ( 'NONE', #18640, #21821, #7111, .T. ) ;
#21100 = CARTESIAN_POINT ( 'NONE',  ( -23.61758233950000019, 37.78045452579999619, -140.0909254550000185 ) ) ;
#21101 = ADVANCED_FACE ( 'NONE', ( #14607 ), #2967, .F. ) ;
#21102 = DIRECTION ( 'NONE',  ( -3.882490197650000213E-51, 1.000000000000000000, 4.009147065150000317E-51 ) ) ;
#21103 = DIRECTION ( 'NONE',  ( -0.1000233216789610108, -0.9949850929136110356, 3.564252608777523239E-13 ) ) ;
#21104 = CARTESIAN_POINT ( 'NONE',  ( 8.288471959293929103, 38.48538972801363656, -142.0444128376232129 ) ) ;
#21105 = AXIS2_PLACEMENT_3D ( 'NONE', #6772, #2982, #19157 ) ;
#21106 = DIRECTION ( 'NONE',  ( 1.000000000000000000, 0.000000000000000000, -2.258609965721802837E-12 ) ) ;
#21107 = EDGE_CURVE ( 'NONE', #9912, #11605, #564, .T. ) ;
#21108 = CARTESIAN_POINT ( 'NONE',  ( -32.50000000000000000, 10.25000000000000000, -149.5552959529999839 ) ) ;
#21109 = CARTESIAN_POINT ( 'NONE',  ( 9.295843182377716118, -34.38416640352239284, -150.0552959530000123 ) ) ;
#21110 = ORIENTED_EDGE ( 'NONE', *, *, #229, .T. ) ;
#21111 = CARTESIAN_POINT ( 'NONE',  ( 11.00000000010000001, 37.00000000000000000, -148.0552959529999839 ) ) ;
#21112 = FILL_AREA_STYLE ('',( #2904 ) ) ;
#21113 = VERTEX_POINT ( 'NONE', #9338 ) ;
#21114 = CARTESIAN_POINT ( 'NONE',  ( -8.309953467263280658, 35.25464643872108184, -140.3668538350108008 ) ) ;
#21115 = CARTESIAN_POINT ( 'NONE',  ( 4.499999999879999102, -3.500000000000000000, -135.0552959530000123 ) ) ;
#21116 = CARTESIAN_POINT ( 'NONE',  ( -6.320468577110000652, -16.70961797440000041, -147.0552959529999839 ) ) ;
#21117 = ORIENTED_EDGE ( 'NONE', *, *, #20659, .F. ) ;
#21118 = CARTESIAN_POINT ( 'NONE',  ( 31.96891336220000213, -40.94938100119999547, -149.8052959529999839 ) ) ;
#21119 = DIRECTION ( 'NONE',  ( 0.000000000000000000, 1.000000000000000000, 0.000000000000000000 ) ) ;
#21120 = VECTOR ( 'NONE', #16823, 1000.000000000000000 ) ;
#21121 = EDGE_CURVE ( 'NONE', #14075, #6301, #14714, .T. ) ;
#21122 = VECTOR ( 'NONE', #4820, 1000.000000000000000 ) ;
#21123 = ORIENTED_EDGE ( 'NONE', *, *, #22496, .T. ) ;
#21124 = CARTESIAN_POINT ( 'NONE',  ( 8.100000000049998761, 37.00000000000000000, -149.5552959529999839 ) ) ;
#21125 = CARTESIAN_POINT ( 'NONE',  ( -17.75130813170000366, 41.00325609940000504, -141.6328284839999867 ) ) ;
#21126 = DIRECTION ( 'NONE',  ( -1.000000000000000000, 0.000000000000000000, 2.257018101830000309E-12 ) ) ;
#21127 = CARTESIAN_POINT ( 'NONE',  ( -20.60824191589999899, -32.00000000000000000, -141.0657682190000060 ) ) ;
#21128 = LINE ( 'NONE', #12063, #12364 ) ;
#21129 = CARTESIAN_POINT ( 'NONE',  ( -25.54709891127356158, 36.13246793439832061, -139.7173810941668251 ) ) ;
#21130 = CARTESIAN_POINT ( 'NONE',  ( 3.611688725869999975E-11, 19.50000000000000000, -136.0552959530000123 ) ) ;
#21131 = EDGE_CURVE ( 'NONE', #903, #13274, #5671, .T. ) ;
#21132 = CYLINDRICAL_SURFACE ( 'NONE', #19586, 14.99999999999999467 ) ;
#21133 = ORIENTED_EDGE ( 'NONE', *, *, #2533, .T. ) ;
#21134 = AXIS2_PLACEMENT_3D ( 'NONE', #22827, #13654, #8289 ) ;
#21135 = CARTESIAN_POINT ( 'NONE',  ( -23.13005137196992678, 38.99857027944433696, -139.6437547635814553 ) ) ;
#21136 = VECTOR ( 'NONE', #20015, 1000.000000000000000 ) ;
#21137 = UNCERTAINTY_MEASURE_WITH_UNIT (LENGTH_MEASURE( 1.000000000000000082E-05 ), #15748, 'distance_accuracy_value', 'NONE');
#21139 = ORIENTED_EDGE ( 'NONE', *, *, #9532, .F. ) ;
#21138 = PRODUCT_RELATED_PRODUCT_CATEGORY ( 'part', '', ( #11988 ) ) ;
#21140 =( NAMED_UNIT ( * ) PLANE_ANGLE_UNIT ( ) SI_UNIT ( $, .RADIAN. ) );
#21141 = ORIENTED_EDGE ( 'NONE', *, *, #17973, .T. ) ;
#21142 = EDGE_CURVE ( 'NONE', #23125, #3916, #22326, .T. ) ;
#21143 = VERTEX_POINT ( 'NONE', #13272 ) ;
#21144 = CARTESIAN_POINT ( 'NONE',  ( 2.742437130648935018, 27.00952979664098308, -136.0552959530062083 ) ) ;
#21145 = DIRECTION ( 'NONE',  ( 0.000000000000000000, 1.000000000000000000, 0.000000000000000000 ) ) ;
#21146 = ORIENTED_EDGE ( 'NONE', *, *, #8404, .F. ) ;
#21147 = ORIENTED_EDGE ( 'NONE', *, *, #18997, .T. ) ;
#21148 = CARTESIAN_POINT ( 'NONE',  ( -15.00000000000000000, -43.00000000000000000, -140.0552959529999839 ) ) ;
#21149 = DIRECTION ( 'NONE',  ( -2.257144641399999941E-12, 4.009147065140000298E-51, -1.000000000000000000 ) ) ;
#21150 = CARTESIAN_POINT ( 'NONE',  ( -10.53621254372777472, 37.95353954631509907, -139.9724837675152571 ) ) ;
#21151 = DIRECTION ( 'NONE',  ( 1.000000000000000000, 0.000000000000000000, -2.257453483404485639E-12 ) ) ;
#21152 = CARTESIAN_POINT ( 'NONE',  ( -8.271665395881317551, 36.97019838859678487, -139.4157638768425613 ) ) ;
#21153 = ADVANCED_FACE ( 'NONE', ( #323 ), #4120, .T. ) ;
#21154 = DIRECTION ( 'NONE',  ( -2.258193632089999862E-12, 0.000000000000000000, -1.000000000000000000 ) ) ;
#21155 = ORIENTED_EDGE ( 'NONE', *, *, #6889, .T. ) ;
#21156 = CARTESIAN_POINT ( 'NONE',  ( -15.00000000000000000, -43.00000000000000000, -137.0552959530000123 ) ) ;
#21157 = VECTOR ( 'NONE', #1021, 1000.000000000000000 ) ;
#21158 = B_SPLINE_CURVE_WITH_KNOTS ( 'NONE', 1,
 ( #7116, #12815 ),
 .UNSPECIFIED., .F., .F.,
 ( 2, 2 ),
 ( -8.099639781640000535, 8.099639781640000535 ),
 .UNSPECIFIED. ) ;
#21159 = LINE ( 'NONE', #12440, #3773 ) ;
#21160 = LINE ( 'NONE', #17104, #17069 ) ;
#21161 = EDGE_CURVE ( 'NONE', #7656, #16174, #2581, .T. ) ;
#21162 = ORIENTED_EDGE ( 'NONE', *, *, #18288, .T. ) ;
#21163 = CARTESIAN_POINT ( 'NONE',  ( -1.844824604570000082, -14.10750774809999974, -148.5552959529999839 ) ) ;
#21164 = VERTEX_POINT ( 'NONE', #13393 ) ;
#21165 =( NAMED_UNIT ( * ) PLANE_ANGLE_UNIT ( ) SI_UNIT ( $, .RADIAN. ) );
#21166 = DIRECTION ( 'NONE',  ( 0.000000000000000000, 1.000000000000000000, 0.000000000000000000 ) ) ;
#21167 = ORIENTED_EDGE ( 'NONE', *, *, #21302, .F. ) ;
#21168 = LINE ( 'NONE', #13898, #7952 ) ;
#21169 = DIRECTION ( 'NONE',  ( 0.000000000000000000, -1.000000000000000000, 0.000000000000000000 ) ) ;
#21170 = VERTEX_POINT ( 'NONE', #11593 ) ;
#21171 = CARTESIAN_POINT ( 'NONE',  ( -14.88943025167819201, 39.58359338906777936, -140.3712910920068566 ) ) ;
#21172 = EDGE_CURVE ( 'NONE', #8089, #12120, #6142, .T. ) ;
#21173 = AXIS2_PLACEMENT_3D ( 'NONE', #18144, #11099, #5635 ) ;
#21174 = CARTESIAN_POINT ( 'NONE',  ( -25.80805072497740227, 36.03780844042944409, -139.4223974946287967 ) ) ;
#21175 = EDGE_LOOP ( 'NONE', ( #20403, #20143, #11310, #16849 ) ) ;
#21176 =( NAMED_UNIT ( * ) SI_UNIT ( $, .STERADIAN. ) SOLID_ANGLE_UNIT ( ) );
#21177 = ORIENTED_EDGE ( 'NONE', *, *, #25, .T. ) ;
#21178 = CARTESIAN_POINT ( 'NONE',  ( -11.38486064709999823, 36.95668670079999885, -140.3965526140000009 ) ) ;
#21179 = DIRECTION ( 'NONE',  ( 0.000000000000000000, 1.000000000000000000, 0.000000000000000000 ) ) ;
#21180 = ORIENTED_EDGE ( 'NONE', *, *, #4173, .T. ) ;
#21181 = CARTESIAN_POINT ( 'NONE',  ( 13.13369214859999978, -50.50000000000000000, -137.0552959530000123 ) ) ;
#21182 = EDGE_CURVE ( 'NONE', #8499, #15103, #10166, .T. ) ;
#21183 = LINE ( 'NONE', #10439, #343 ) ;
#21184 = EDGE_CURVE ( 'NONE', #9674, #1369, #12878, .T. ) ;
#21185 = DIRECTION ( 'NONE',  ( 0.000000000000000000, -1.000000000000000000, 0.000000000000000000 ) ) ;
#21186 = EDGE_CURVE ( 'NONE', #15988, #2866, #4593, .T. ) ;
#21187 = CIRCLE ( 'NONE', #10131, 2.999999999999999112 ) ;
#21188 = EDGE_CURVE ( 'NONE', #6545, #11025, #6035, .T. ) ;
#21189 = VECTOR ( 'NONE', #12984, 1000.000000000000000 ) ;
#21190 = EDGE_LOOP ( 'NONE', ( #10376, #16547, #7166, #5011 ) ) ;
#21191 = LINE ( 'NONE', #1083, #14296 ) ;
#21192 = DIRECTION ( 'NONE',  ( -1.000000000000000000, 0.000000000000000000, 0.000000000000000000 ) ) ;
#21193 = CARTESIAN_POINT ( 'NONE',  ( -13.56475956976288444, 38.79166783126999007, -140.1832272770149643 ) ) ;
#21194 = CARTESIAN_POINT ( 'NONE',  ( 25.04148309045456955, -26.71426189482850333, -147.5552959530288035 ) ) ;
#21195 = ORIENTED_EDGE ( 'NONE', *, *, #8235, .F. ) ;
#21196 = CARTESIAN_POINT ( 'NONE',  ( 6.500000000040000003, 13.00000000000000000, -136.0552959530000123 ) ) ;
#21197 = CARTESIAN_POINT ( 'NONE',  ( -33.50000000000000000, 26.00000000000000000, -146.5552959529999839 ) ) ;
#21198 = CARTESIAN_POINT ( 'NONE',  ( -32.50000000000000000, 47.50000000000000000, -136.0552959530000123 ) ) ;
#21199 = DIRECTION ( 'NONE',  ( 2.507554887169999917E-12, 0.000000000000000000, -1.000000000000000000 ) ) ;
#21200 = CARTESIAN_POINT ( 'NONE',  ( -35.73252798949999942, 37.00000000000000000, -140.5552959529999839 ) ) ;
#21201 = VERTEX_POINT ( 'NONE', #1034 ) ;
#21202 = LINE ( 'NONE', #18932, #16016 ) ;
#21203 = VECTOR ( 'NONE', #8087, 1000.000000000000000 ) ;
#21204 = CARTESIAN_POINT ( 'NONE',  ( -9.434278515689999978, -18.41834002140000237, -147.5552959529999839 ) ) ;
#21205 = COLOUR_RGB ( '', 0.08235294, 0.09019608, 0.10196078) ;
#21206 = DIRECTION ( 'NONE',  ( 1.000000000000000000, 0.000000000000000000, 0.000000000000000000 ) ) ;
#21207 = CARTESIAN_POINT ( 'NONE',  ( -16.20111387579999729, -1.500000000000000000, -147.8591802640000026 ) ) ;
#21208 = CARTESIAN_POINT ( 'NONE',  ( 9.183200060760000838, -6.500000000000000000, -148.5552959529999839 ) ) ;
#21209 = VERTEX_POINT ( 'NONE', #21022 ) ;
#21210 = DIRECTION ( 'NONE',  ( 2.257157423930000049E-12, 0.000000000000000000, 1.000000000000000000 ) ) ;
#21211 = ADVANCED_FACE ( 'NONE', ( #15665 ), #6370, .F. ) ;
#21212 = CARTESIAN_POINT ( 'NONE',  ( 5.257235470750120321, -2.190481511161879169, -150.0552959529999839 ) ) ;
#21213 = ORIENTED_EDGE ( 'NONE', *, *, #18981, .F. ) ;
#21214 = CARTESIAN_POINT ( 'NONE',  ( -28.67645553090000021, 33.79622934780000065, -142.1760638819999940 ) ) ;
#21215 = DIRECTION ( 'NONE',  ( 1.000000000000000000, -5.094701932209999624E-24, -2.257144641399999941E-12 ) ) ;
#21216 = ORIENTED_EDGE ( 'NONE', *, *, #20092, .T. ) ;
#21217 = CARTESIAN_POINT ( 'NONE',  ( -23.42774316933405387, 40.39856899166812099, -146.1482362793011021 ) ) ;
#21218 = AXIS2_PLACEMENT_3D ( 'NONE', #4215, #22072, #2444 ) ;
#21219 = CARTESIAN_POINT ( 'NONE',  ( 2.218297500549999857, -15.44723318490000175, -147.5552959529999839 ) ) ;
#21220 = DIRECTION ( 'NONE',  ( 1.000000000000000000, 0.000000000000000000, 0.000000000000000000 ) ) ;
#21221 = DIRECTION ( 'NONE',  ( -0.07970438983373200059, -0.9968185442904001770, 8.268372250843320857E-13 ) ) ;
#21222 = ORIENTED_EDGE ( 'NONE', *, *, #1963, .T. ) ;
#21223 = CARTESIAN_POINT ( 'NONE',  ( -10.51637644729841092, 32.80416691061421375, -146.2924636027869383 ) ) ;
#21224 = LINE ( 'NONE', #21108, #22252 ) ;
#21225 = CARTESIAN_POINT ( 'NONE',  ( -8.436279545364561372, 40.51610847932013826, -146.1280570644845511 ) ) ;
#21226 = LINE ( 'NONE', #17079, #16752 ) ;
#21227 = VERTEX_POINT ( 'NONE', #8030 ) ;
#21228 = SURFACE_SIDE_STYLE ('',( #6346 ) ) ;
#21229 = EDGE_LOOP ( 'NONE', ( #21213, #13895, #7351, #11378 ) ) ;
#21230 = CARTESIAN_POINT ( 'NONE',  ( -7.231565869921675827, 33.87808888013704944, -142.3031534620325260 ) ) ;
#21231 = CARTESIAN_POINT ( 'NONE',  ( -29.78377644599999741, 41.56884167520000517, -144.3599435680000056 ) ) ;
#21232 = CARTESIAN_POINT ( 'NONE',  ( -21.80913741070000000, 38.74859698539999897, -147.9243209519999880 ) ) ;
#21233 = AXIS2_PLACEMENT_3D ( 'NONE', #2287, #13089, #3942 ) ;
#21234 = VECTOR ( 'NONE', #4365, 1000.000000000000000 ) ;
#21235 = ORIENTED_EDGE ( 'NONE', *, *, #9133, .F. ) ;
#21236 = EDGE_CURVE ( 'NONE', #21893, #3677, #19339, .T. ) ;
#21237 = CARTESIAN_POINT ( 'NONE',  ( 0.000000000000000000, 0.000000000000000000, -150.0552959529999839 ) ) ;
#21238 = CARTESIAN_POINT ( 'NONE',  ( 25.22833163479999996, -45.34299735780000162, -149.5552959529999839 ) ) ;
#21239 = AXIS2_PLACEMENT_3D ( 'NONE', #9265, #9372, #16645 ) ;
#21240 = ORIENTED_EDGE ( 'NONE', *, *, #7468, .T. ) ;
#21241 = LINE ( 'NONE', #4577, #19797 ) ;
#21242 = AXIS2_PLACEMENT_3D ( 'NONE', #7031, #21687, #18342 ) ;
#21243 = CARTESIAN_POINT ( 'NONE',  ( 17.57650987475626891, 23.28094649260091842, -150.0552959529999839 ) ) ;
#21244 = CARTESIAN_POINT ( 'NONE',  ( 6.500000000159999125, 20.50000000000000000, -140.5552959529999839 ) ) ;
#21245 = PLANE ( 'NONE',  #3815 ) ;
#21246 = CARTESIAN_POINT ( 'NONE',  ( -34.50000000000000000, 48.00000000000000000, -141.5552959529999839 ) ) ;
#21247 = CARTESIAN_POINT ( 'NONE',  ( -15.57786843150000067, 37.00666880280000726, -148.5521201120000114 ) ) ;
#21248 = CARTESIAN_POINT ( 'NONE',  ( 5.257167980435379029, -4.809692093865743701, -150.0552959530000123 ) ) ;
#21249 = DIRECTION ( 'NONE',  ( 1.000000000000000000, 0.000000000000000000, 0.000000000000000000 ) ) ;
#21250 = AXIS2_PLACEMENT_3D ( 'NONE', #19459, #23372, #3263 ) ;
#21251 = VECTOR ( 'NONE', #888, 1000.000000000000114 ) ;
#21252 = ORIENTED_EDGE ( 'NONE', *, *, #16126, .F. ) ;
#21253 = LINE ( 'NONE', #19341, #21630 ) ;
#21254 = AXIS2_PLACEMENT_3D ( 'NONE', #842, #20698, #18684 ) ;
#21255 = EDGE_LOOP ( 'NONE', ( #12012, #18561, #8443, #7304 ) ) ;
#21256 = VECTOR ( 'NONE', #5192, 1000.000000000000000 ) ;
#21257 = ORIENTED_EDGE ( 'NONE', *, *, #16320, .F. ) ;
#21258 = DIRECTION ( 'NONE',  ( 0.000000000000000000, 0.000000000000000000, 1.000000000000000000 ) ) ;
#21259 = CARTESIAN_POINT ( 'NONE',  ( -28.36041799518341833, 33.90485755864479955, -142.1995097533358319 ) ) ;
#21260 = ORIENTED_EDGE ( 'NONE', *, *, #13911, .F. ) ;
#21261 = ORIENTED_EDGE ( 'NONE', *, *, #15345, .T. ) ;
#21262 = EDGE_CURVE ( 'NONE', #11453, #19376, #17439, .T. ) ;
#21263 = CARTESIAN_POINT ( 'NONE',  ( -20.60824191589999899, -4.000000000000000000, -144.8157682190000060 ) ) ;
#21264 = CARTESIAN_POINT ( 'NONE',  ( -19.10036854000342998, 37.06903765909164861, -148.2030617969362538 ) ) ;
#21265 = CARTESIAN_POINT ( 'NONE',  ( -11.74549879742581204, 39.03442698418600543, -147.0603333942009101 ) ) ;
#21266 = EDGE_CURVE ( 'NONE', #7656, #20624, #9807, .T. ) ;
#21267 = DIRECTION ( 'NONE',  ( -2.257198259660000092E-12, 0.000000000000000000, -1.000000000000000000 ) ) ;
#21268 = CARTESIAN_POINT ( 'NONE',  ( -7.530507654992796951, 34.12260748990723869, -140.1991143277646188 ) ) ;
#21269 = VECTOR ( 'NONE', #20678, 1000.000000000000227 ) ;
#21270 = ORIENTED_EDGE ( 'NONE', *, *, #23514, .F. ) ;
#21271 = VECTOR ( 'NONE', #22235, 1000.000000000000000 ) ;
#21272 = LINE ( 'NONE', #6269, #3371 ) ;
#21273 = AXIS2_PLACEMENT_3D ( 'NONE', #7690, #13164, #4127 ) ;
#21274 = CARTESIAN_POINT ( 'NONE',  ( 5.960959015012474715, -3.892621826538923191, -136.0552959530033377 ) ) ;
#21275 = VECTOR ( 'NONE', #13, 1000.000000000000000 ) ;
#21276 = DIRECTION ( 'NONE',  ( -1.211690350419999855E-27, -2.765629237170000203E-27, 1.000000000000000000 ) ) ;
#21277 = ORIENTED_EDGE ( 'NONE', *, *, #4435, .F. ) ;
#21278 = LINE ( 'NONE', #5195, #18663 ) ;
#21279 = ORIENTED_EDGE ( 'NONE', *, *, #554, .T. ) ;
#21280 = DIRECTION ( 'NONE',  ( -4.430318231639999944E-12, 6.100259101500000139E-13, -1.000000000000000000 ) ) ;
#21281 = CARTESIAN_POINT ( 'NONE',  ( 25.02856554857857674, -26.78821141716894871, -146.5552959529967154 ) ) ;
#21282 = ADVANCED_FACE ( 'NONE', ( #19108 ), #4471, .T. ) ;
#21283 = VERTEX_POINT ( 'NONE', #22445 ) ;
#21284 = CARTESIAN_POINT ( 'NONE',  ( -19.39325354309108818, 37.07505107991995175, -139.9601895475230151 ) ) ;
#21285 = DIRECTION ( 'NONE',  ( -2.257144641399999941E-12, 0.000000000000000000, -1.000000000000000000 ) ) ;
#21286 = ORIENTED_EDGE ( 'NONE', *, *, #18480, .T. ) ;
#21287 = DIRECTION ( 'NONE',  ( 0.000000000000000000, 0.000000000000000000, 1.000000000000000000 ) ) ;
#21288 = CARTESIAN_POINT ( 'NONE',  ( -24.36912841275935904, 34.40976477778183806, -147.5507798122575878 ) ) ;
#21289 = VERTEX_POINT ( 'NONE', #2811 ) ;
#21290 = VECTOR ( 'NONE', #23209, 1000.000000000000114 ) ;
#21291 = VECTOR ( 'NONE', #3153, 1000.000000000000000 ) ;
#21292 = VERTEX_POINT ( 'NONE', #8263 ) ;
#21293 = AXIS2_PLACEMENT_3D ( 'NONE', #7454, #14717, #5673 ) ;
#21294 = CARTESIAN_POINT ( 'NONE',  ( -12.57385931489999997, 38.47543513199999410, -147.4253642439999794 ) ) ;
#21295 = CIRCLE ( 'NONE', #3817, 1.000000000000000888 ) ;
#21296 = CARTESIAN_POINT ( 'NONE',  ( -2.499999999929999994, 42.50000000000000000, -138.0552959530000123 ) ) ;
#21297 = ORIENTED_EDGE ( 'NONE', *, *, #16367, .F. ) ;
#21298 = EDGE_CURVE ( 'NONE', #18790, #17304, #13246, .T. ) ;
#21299 = DIRECTION ( 'NONE',  ( 4.430318231639999944E-12, -6.100259101500000139E-13, 1.000000000000000000 ) ) ;
#21300 = DIRECTION ( 'NONE',  ( -1.457881434569999917E-12, -1.723066134159999823E-12, 1.000000000000000000 ) ) ;
#21301 = LINE ( 'NONE', #6649, #8278 ) ;
#21302 = EDGE_CURVE ( 'NONE', #9978, #12270, #10041, .T. ) ;
#21303 = ORIENTED_EDGE ( 'NONE', *, *, #1398, .T. ) ;
#21304 = VECTOR ( 'NONE', #5178, 1000.000000000000000 ) ;
#21305 =( GEOMETRIC_REPRESENTATION_CONTEXT ( 3 ) GLOBAL_UNCERTAINTY_ASSIGNED_CONTEXT ( ( #18271 ) ) GLOBAL_UNIT_ASSIGNED_CONTEXT ( ( #18596, #20626, #14676 ) ) REPRESENTATION_CONTEXT ( 'NONE', 'WORKASPACE' ) );
#21306 = DIRECTION ( 'NONE',  ( -1.000000000000000000, 0.000000000000000000, 0.000000000000000000 ) ) ;
#21307 = LINE ( 'NONE', #8194, #12730 ) ;
#21308 = CARTESIAN_POINT ( 'NONE',  ( -14.18713694461474439, 40.16576858557153429, -142.2514428343604038 ) ) ;
#21309 = CARTESIAN_POINT ( 'NONE',  ( -28.90798551748587641, 37.01360947634927356, -139.5686590453487952 ) ) ;
#21310 = VERTEX_POINT ( 'NONE', #11954 ) ;
#21311 = DIRECTION ( 'NONE',  ( -2.842170943040000002E-14, -3.552713678800000097E-13, -1.000000000000000000 ) ) ;
#21312 = LINE ( 'NONE', #21430, #18444 ) ;
#21313 = EDGE_CURVE ( 'NONE', #17988, #1030, #22529, .T. ) ;
#21314 = CARTESIAN_POINT ( 'NONE',  ( 3.780861691979999772, -4.816373842840000030, -143.0552959529999839 ) ) ;
#21315 = CARTESIAN_POINT ( 'NONE',  ( -38.72222222220000276, 26.50000000000000000, -140.5552959529999839 ) ) ;
#21316 = CARTESIAN_POINT ( 'NONE',  ( -23.90890255121786367, 36.92681688281093955, -147.8857207493851433 ) ) ;
#21317 = CARTESIAN_POINT ( 'NONE',  ( 25.00000852249999994, -26.83294714660000224, -142.5552959529999839 ) ) ;
#21318 = ADVANCED_FACE ( 'NONE', ( #2320 ), #1312, .F. ) ;
#21319 = ORIENTED_EDGE ( 'NONE', *, *, #10682, .T. ) ;
#21320 = CARTESIAN_POINT ( 'NONE',  ( -16.92431971699136994, 37.01165972488241351, -139.4624774945036449 ) ) ;
#21321 = EDGE_CURVE ( 'NONE', #15557, #12276, #17284, .T. ) ;
#21322 = LINE ( 'NONE', #13931, #6037 ) ;
#21323 = ADVANCED_FACE ( 'NONE', ( #2780 ), #7808, .F. ) ;
#21324 = CARTESIAN_POINT ( 'NONE',  ( -5.459597139497688545, 36.94776568913771797, -139.8191173758904142 ) ) ;
#21325 = CARTESIAN_POINT ( 'NONE',  ( -7.107905118369999720, 36.22301459080000541, -148.1570340890000068 ) ) ;
#21326 = DIRECTION ( 'NONE',  ( 0.2024296638729825848, 0.9792968044389154247, -3.528679552389696828E-13 ) ) ;
#21327 = STYLED_ITEM ( 'NONE', ( #20871 ), #11815 ) ;
#21328 = ORIENTED_EDGE ( 'NONE', *, *, #13026, .T. ) ;
#21329 = PLANE ( 'NONE',  #21014 ) ;
#21330 = CARTESIAN_POINT ( 'NONE',  ( -25.27079369000000142, 34.74837955689999802, -147.2605407199999945 ) ) ;
#21331 = ORIENTED_EDGE ( 'NONE', *, *, #15036, .F. ) ;
#21332 = B_SPLINE_CURVE_WITH_KNOTS ( 'NONE', 5,
 ( #3245, #6809, #1249, #3023, #13840, #1354, #4915, #19077, #22645, #8579, #23001, #12040 ),
 .UNSPECIFIED., .F., .F.,
 ( 6, 3, 3, 6 ),
 ( 0.000000000000000000, 4.445608688430000122, 8.917804078430000558, 13.41780914199999941 ),
 .UNSPECIFIED. ) ;
#21333 = B_SPLINE_CURVE_WITH_KNOTS ( 'NONE', 3,
 ( #10022, #19450, #14089, #12051, #10490, #19321 ),
 .UNSPECIFIED., .F., .F.,
 ( 4, 2, 4 ),
 ( 0.000000000000000000, 0.5000000000000000000, 1.000000000000000000 ),
 .UNSPECIFIED. ) ;
#21334 = CARTESIAN_POINT ( 'NONE',  ( -29.32420091883213331, 34.33926911055133502, -140.4578922366215465 ) ) ;
#21335 = DIRECTION ( 'NONE',  ( 1.000000000000000000, 0.000000000000000000, 0.000000000000000000 ) ) ;
#21336 = ORIENTED_EDGE ( 'NONE', *, *, #6044, .T. ) ;
#21337 = EDGE_CURVE ( 'NONE', #12661, #5687, #7279, .T. ) ;
#21338 = CARTESIAN_POINT ( 'NONE',  ( -23.71327735677587611, 38.51283207398868313, -147.7059059786899979 ) ) ;
#21339 = CARTESIAN_POINT ( 'NONE',  ( -33.50000000000000000, 48.00000000000000000, -146.5552959529999839 ) ) ;
#21340 = CARTESIAN_POINT ( 'NONE',  ( -10.49999999989999822, 37.00000000000000000, -144.0552959529999839 ) ) ;
#21341 = CARTESIAN_POINT ( 'NONE',  ( 7.672998245282296459, 38.25143462710926912, -141.8910607812413502 ) ) ;
#21342 = ORIENTED_EDGE ( 'NONE', *, *, #14639, .T. ) ;
#21343 = CARTESIAN_POINT ( 'NONE',  ( -10.35239533838411852, 35.24123622976342318, -147.9781929050253382 ) ) ;
#21344 = CIRCLE ( 'NONE', #22868, 5.000000000000000000 ) ;
#21345 = LINE ( 'NONE', #8474, #23387 ) ;
#21346 = AXIS2_PLACEMENT_3D ( 'NONE', #5534, #21615, #298 ) ;
#21347 = EDGE_CURVE ( 'NONE', #15836, #19038, #8689, .T. ) ;
#21348 = CARTESIAN_POINT ( 'NONE',  ( -46.50000000000000000, 47.50000000000000000, -149.0552959529999839 ) ) ;
#21349 = DIRECTION ( 'NONE',  ( -2.043390161445605165E-12, 0.000000000000000000, -1.000000000000000000 ) ) ;
#21350 = ORIENTED_EDGE ( 'NONE', *, *, #14864, .T. ) ;
#21351 = EDGE_CURVE ( 'NONE', #9207, #17699, #12271, .T. ) ;
#21352 = CARTESIAN_POINT ( 'NONE',  ( 23.50000000000000000, -20.50000000000000000, -137.2152959530000089 ) ) ;
#21353 = APPLICATION_CONTEXT ( 'automotive_design' ) ;
#21354 = ORIENTED_EDGE ( 'NONE', *, *, #7117, .T. ) ;
#21355 = CARTESIAN_POINT ( 'NONE',  ( -7.549714246211497226, 33.73496036356508654, -146.1021208403070091 ) ) ;
#21356 = CARTESIAN_POINT ( 'NONE',  ( -6.183234097709999766, 41.28010592229999531, -143.5033826240000110 ) ) ;
#21357 = CARTESIAN_POINT ( 'NONE',  ( 24.87050155979999744, -26.86223000240000047, -146.5552959529999839 ) ) ;
#21358 = ORIENTED_EDGE ( 'NONE', *, *, #15933, .T. ) ;
#21359 = PLANE ( 'NONE',  #9487 ) ;
#21360 = CARTESIAN_POINT ( 'NONE',  ( 32.50000000000000000, 32.96379895129999937, -136.0552959530000123 ) ) ;
#21361 = VECTOR ( 'NONE', #6782, 1000.000000000000000 ) ;
#21362 = VECTOR ( 'NONE', #21938, 1000.000000000000000 ) ;
#21363 = VERTEX_POINT ( 'NONE', #14185 ) ;
#21364 = VECTOR ( 'NONE', #10235, 1000.000000000000000 ) ;
#21365 = CARTESIAN_POINT ( 'NONE',  ( -16.81794493339999619, 37.02435727940000731, -140.5111119820000170 ) ) ;
#21366 = CARTESIAN_POINT ( 'NONE',  ( 2.499999999879999990, -3.000000000000000000, -135.2552959529999725 ) ) ;
#21367 = CARTESIAN_POINT ( 'NONE',  ( -12.07808196999505412, -42.21475634692215806, -150.0552959529999839 ) ) ;
#21368 = DIRECTION ( 'NONE',  ( -1.000000000000000000, 1.190078432789999897E-50, 2.257144641399999941E-12 ) ) ;
#21369 = LINE ( 'NONE', #1499, #10455 ) ;
#21370 = DIRECTION ( 'NONE',  ( 1.527666881879999979E-13, 8.171241461240000022E-13, 1.000000000000000000 ) ) ;
#21371 = ITEM_DEFINED_TRANSFORMATION ( 'NONE', 'NONE', #1291,  #5025 ) ;
#21372 = DIRECTION ( 'NONE',  ( 4.510774274160000731E-12, -1.321907670990000086E-13, 1.000000000000000000 ) ) ;
#21373 = CARTESIAN_POINT ( 'NONE',  ( -2.270906560010169883, 42.90066631520362250, -136.0552959530027408 ) ) ;
#21374 = EDGE_CURVE ( 'NONE', #3905, #6268, #7555, .T. ) ;
#21375 = ORIENTED_EDGE ( 'NONE', *, *, #23203, .F. ) ;
#21376 = EDGE_CURVE ( 'NONE', #467, #12707, #17750, .T. ) ;
#21377 =( GEOMETRIC_REPRESENTATION_CONTEXT ( 3 ) GLOBAL_UNCERTAINTY_ASSIGNED_CONTEXT ( ( #15882 ) ) GLOBAL_UNIT_ASSIGNED_CONTEXT ( ( #6140, #13758, #21609 ) ) REPRESENTATION_CONTEXT ( 'NONE', 'WORKASPACE' ) );
#21378 = UNCERTAINTY_MEASURE_WITH_UNIT (LENGTH_MEASURE( 1.000000000000000082E-05 ), #13664, 'distance_accuracy_value', 'NONE');
#21379 = VECTOR ( 'NONE', #22454, 1000.000000000000000 ) ;
#21380 = EDGE_LOOP ( 'NONE', ( #14203, #5126, #527, #6282 ) ) ;
#21381 = SHAPE_REPRESENTATION_RELATIONSHIP ( 'NONE' , 'NONE' ,  #15114, #3292 ) ;
#21382 = EDGE_LOOP ( 'NONE', ( #14929, #15800, #20367, #13855, #14490, #15778 ) ) ;
#21383 = DIRECTION ( 'NONE',  ( 0.000000000000000000, -1.000000000000000000, 0.000000000000000000 ) ) ;
#21384 = DIRECTION ( 'NONE',  ( 1.000000000000000000, 0.000000000000000000, -1.527536832333224173E-13 ) ) ;
#21385 = LINE ( 'NONE', #3639, #12970 ) ;
#21386 = ORIENTED_EDGE ( 'NONE', *, *, #6482, .F. ) ;
#21387 = CARTESIAN_POINT ( 'NONE',  ( -4.576509874761471863, 21.71905350741746332, -150.0552959529999839 ) ) ;
#21388 = CARTESIAN_POINT ( 'NONE',  ( -19.38605492679999998, 35.40602226210000225, -140.5130341980000139 ) ) ;
#21389 = CARTESIAN_POINT ( 'NONE',  ( -12.14203431770015484, 38.98285737023589093, -146.9062848651227853 ) ) ;
#21390 = DIRECTION ( 'NONE',  ( 1.000000000000000000, 0.000000000000000000, -2.259303855112193156E-12 ) ) ;
#21391 = CARTESIAN_POINT ( 'NONE',  ( -8.168738184452987383, 35.97421812808207164, -139.4219941368502305 ) ) ;
#21392 = VERTEX_POINT ( 'NONE', #1465 ) ;
#21393 = CARTESIAN_POINT ( 'NONE',  ( 9.771538001791512329, 36.20254759283128010, -141.6854458089526645 ) ) ;
#21394 = VECTOR ( 'NONE', #6322, 1000.000000000000000 ) ;
#21395 = CARTESIAN_POINT ( 'NONE',  ( 25.31684607429999900, -45.26810052439999765, -150.0552959529999839 ) ) ;
#21396 = DIRECTION ( 'NONE',  ( 0.000000000000000000, 0.000000000000000000, -1.000000000000000000 ) ) ;
#21397 = ORIENTED_EDGE ( 'NONE', *, *, #2717, .T. ) ;
#21398 = EDGE_CURVE ( 'NONE', #567, #7407, #1881, .T. ) ;
#21399 = CARTESIAN_POINT ( 'NONE',  ( -3.500000000000000000, 44.50000000000000000, -150.0552959529999839 ) ) ;
#21400 = ORIENTED_EDGE ( 'NONE', *, *, #4786, .F. ) ;
#21401 = CARTESIAN_POINT ( 'NONE',  ( -9.999999999969999109, 19.50000000000000000, -137.0552959530000123 ) ) ;
#21402 = EDGE_CURVE ( 'NONE', #1705, #10837, #3351, .T. ) ;
#21403 = DIRECTION ( 'NONE',  ( -7.483957154334591044E-15, 0.000000000000000000, 1.000000000000000000 ) ) ;
#21404 = ORIENTED_EDGE ( 'NONE', *, *, #6361, .T. ) ;
#21405 = CARTESIAN_POINT ( 'NONE',  ( 8.500000000060001781, 38.50000000000000000, -146.0552959529999839 ) ) ;
#21406 = CARTESIAN_POINT ( 'NONE',  ( -35.47299999999999898, 14.00000000000000000, -144.0552959529999839 ) ) ;
#21407 = ORIENTED_EDGE ( 'NONE', *, *, #6629, .T. ) ;
#21408 = CARTESIAN_POINT ( 'NONE',  ( -15.86641283045871020, 39.36988465981706753, -147.1618092805611013 ) ) ;
#21409 = CARTESIAN_POINT ( 'NONE',  ( 20.40453940470000305, -31.75469340779999428, -143.5552959529999839 ) ) ;
#21410 = EDGE_LOOP ( 'NONE', ( #14471, #10465, #8108, #14011 ) ) ;
#21411 = DIRECTION ( 'NONE',  ( 1.000000000000000000, 0.000000000000000000, 0.000000000000000000 ) ) ;
#21412 = VERTEX_POINT ( 'NONE', #1594 ) ;
#21413 = CARTESIAN_POINT ( 'NONE',  ( 6.500000000000000000, 20.50000000000000000, -150.0552959529999839 ) ) ;
#21414 = PLANE ( 'NONE',  #17584 ) ;
#21415 = ORIENTED_EDGE ( 'NONE', *, *, #2283, .T. ) ;
#21416 = DIRECTION ( 'NONE',  ( -0.06298685227120542907, -0.9980143568310855251, 1.534772309240130738E-13 ) ) ;
#21417 = PLANE ( 'NONE',  #19329 ) ;
#21418 = EDGE_LOOP ( 'NONE', ( #14465, #7960, #16783, #19795 ) ) ;
#21419 = LINE ( 'NONE', #12592, #18959 ) ;
#21420 = PRODUCT_DEFINITION_FORMATION_WITH_SPECIFIED_SOURCE ( 'ANY', '', #10985, .NOT_KNOWN. ) ;
#21421 = EDGE_LOOP ( 'NONE', ( #3807, #9764, #14312, #19523 ) ) ;
#21422 = DIRECTION ( 'NONE',  ( -2.688820921349999492E-17, 1.000000000000000000, 6.069065783950000909E-29 ) ) ;
#21423 = CARTESIAN_POINT ( 'NONE',  ( -34.50000000000000000, 46.00000000000000000, -146.5552959529999839 ) ) ;
#21424 = VECTOR ( 'NONE', #18278, 1000.000000000000000 ) ;
#21425 = CARTESIAN_POINT ( 'NONE',  ( -14.72926790370904904, 38.75043575020603726, -148.1588405132401647 ) ) ;
#21426 = CARTESIAN_POINT ( 'NONE',  ( -28.93621398888856433, 40.40455385674768252, -140.8397343873709531 ) ) ;
#21427 = ORIENTED_EDGE ( 'NONE', *, *, #17136, .T. ) ;
#21428 = DIRECTION ( 'NONE',  ( 4.433786671139999973E-12, -6.110667527539999876E-13, 1.000000000000000000 ) ) ;
#21429 = EDGE_CURVE ( 'NONE', #10756, #12039, #8815, .T. ) ;
#21430 = CARTESIAN_POINT ( 'NONE',  ( 1.133692148650000009, 51.00000000000000000, -137.0552959530000123 ) ) ;
#21431 = DIRECTION ( 'NONE',  ( 2.257144641399999941E-12, -4.009147065140000298E-51, 1.000000000000000000 ) ) ;
#21432 = CARTESIAN_POINT ( 'NONE',  ( 10.68320006080000084, -20.50000000000000000, -148.5552959529999839 ) ) ;
#21433 = CARTESIAN_POINT ( 'NONE',  ( -21.71608528380000180, -1.500000000000000000, -144.8157682190000060 ) ) ;
#21434 = CARTESIAN_POINT ( 'NONE',  ( 9.183200060760000838, -6.500000000000000000, -148.5552959529999839 ) ) ;
#21435 = ORIENTED_EDGE ( 'NONE', *, *, #22890, .F. ) ;
#21436 = LINE ( 'NONE', #16193, #19054 ) ;
#21437 = FACE_OUTER_BOUND ( 'NONE', #4827, .T. ) ;
#21438 = PLANE ( 'NONE',  #2274 ) ;
#21439 = ADVANCED_FACE ( 'NONE', ( #23346 ), #21694, .T. ) ;
#21440 = CARTESIAN_POINT ( 'NONE',  ( -4.726668495498447697, 39.51488736142145797, -140.6795032275781807 ) ) ;
#21441 = CYLINDRICAL_SURFACE ( 'NONE', #863, 0.7500000000000006661 ) ;
#21442 = DIRECTION ( 'NONE',  ( 1.000000000000000000, 0.000000000000000000, -8.954760363766765626E-12 ) ) ;
#21443 = EDGE_LOOP ( 'NONE', ( #1576, #21027, #1072, #17536 ) ) ;
#21444 = AXIS2_PLACEMENT_3D ( 'NONE', #12644, #19915, #10609 ) ;
#21445 = DIRECTION ( 'NONE',  ( 1.000000000000000000, 0.000000000000000000, 2.257144641399999941E-12 ) ) ;
#21446 = CARTESIAN_POINT ( 'NONE',  ( -15.50000000000000000, 21.50000000000000000, -151.0552959529999839 ) ) ;
#21447 = ORIENTED_EDGE ( 'NONE', *, *, #23485, .T. ) ;
#21448 = EDGE_CURVE ( 'NONE', #1104, #21465, #18108, .T. ) ;
#21449 = CARTESIAN_POINT ( 'NONE',  ( 8.982728679470000088, -17.28848751049999777, -144.5552959529999839 ) ) ;
#21450 = EDGE_LOOP ( 'NONE', ( #21146, #7738, #8851, #874, #14998, #15816, #15909, #1304 ) ) ;
#21451 = CARTESIAN_POINT ( 'NONE',  ( -24.00988078544188653, 37.66389269266682049, -147.5188782761057382 ) ) ;
#21452 = ADVANCED_FACE ( 'NONE', ( #35 ), #21812, .T. ) ;
#21453 = CARTESIAN_POINT ( 'NONE',  ( -2.499999999969999998, 37.00000000000000000, -137.0552959530000123 ) ) ;
#21454 = CARTESIAN_POINT ( 'NONE',  ( 4.499999999879999102, -5.500000000000000000, -135.0552959530000123 ) ) ;
#21455 = CARTESIAN_POINT ( 'NONE',  ( 7.250480400028753714, 36.17009463394629876, -141.6970570770266136 ) ) ;
#21456 = ORIENTED_EDGE ( 'NONE', *, *, #13640, .F. ) ;
#21457 = LINE ( 'NONE', #17883, #22312 ) ;
#21458 = PLANE ( 'NONE',  #9313 ) ;
#21459 = CARTESIAN_POINT ( 'NONE',  ( -9.289091550977641276, 37.68670816229094811, -147.3844454406949467 ) ) ;
#21460 = CARTESIAN_POINT ( 'NONE',  ( 3.763193976738810509, -34.16260098204838158, -136.0552959530085388 ) ) ;
#21461 = AXIS2_PLACEMENT_3D ( 'NONE', #3587, #23222, #7029 ) ;
#21462 = VERTEX_POINT ( 'NONE', #3137 ) ;
#21463 = DIRECTION ( 'NONE',  ( 3.994014902950000436E-29, -1.000000000000000000, 4.148443855749999753E-27 ) ) ;
#21464 = ADVANCED_FACE ( 'NONE', ( #4439 ), #13948, .F. ) ;
#21465 = VERTEX_POINT ( 'NONE', #15625 ) ;
#21466 = CARTESIAN_POINT ( 'NONE',  ( -7.506111428101620575, 33.37436714625175682, -146.3147224704404152 ) ) ;
#21467 = FACE_OUTER_BOUND ( 'NONE', #12776, .T. ) ;
#21468 = PLANE ( 'NONE',  #3590 ) ;
#21469 = ADVANCED_FACE ( 'NONE', ( #11922 ), #4913, .F. ) ;
#21470 = ORIENTED_EDGE ( 'NONE', *, *, #8210, .F. ) ;
#21471 = DIRECTION ( 'NONE',  ( -1.000000000000000000, 0.000000000000000000, 0.000000000000000000 ) ) ;
#21472 = LINE ( 'NONE', #5401, #11009 ) ;
#21473 = ORIENTED_EDGE ( 'NONE', *, *, #10111, .T. ) ;
#21474 = CARTESIAN_POINT ( 'NONE',  ( 18.95053822279999878, -50.00000000000000000, -150.0552959529999839 ) ) ;
#21475 = EDGE_CURVE ( 'NONE', #21766, #12998, #18953, .T. ) ;
#21476 = FACE_BOUND ( 'NONE', #6828, .T. ) ;
#21477 = EDGE_CURVE ( 'NONE', #1038, #11485, #10128, .T. ) ;
#21479 = VECTOR ( 'NONE', #20956, 1000.000000000000000 ) ;
#21478 = CARTESIAN_POINT ( 'NONE',  ( -13.15635984007525749, -40.60099947280546928, -150.0552959530000123 ) ) ;
#21480 = LINE ( 'NONE', #21598, #9848 ) ;
#21481 = EDGE_CURVE ( 'NONE', #5331, #19967, #13473, .T. ) ;
#21482 = CARTESIAN_POINT ( 'NONE',  ( 29.68320006080000084, -24.50000000000000000, -150.0552959529999839 ) ) ;
#21483 = EDGE_CURVE ( 'NONE', #22206, #16939, #10367, .T. ) ;
#21484 = CARTESIAN_POINT ( 'NONE',  ( 9.152949117189999484, -16.59780702190000312, -147.5552959529999839 ) ) ;
#21485 = CONTEXT_DEPENDENT_SHAPE_REPRESENTATION ( #20434, #4611 ) ;
#21486 = DIRECTION ( 'NONE',  ( -0.4567501391959232770, 0.5397956190499111351, 0.7071067811858601226 ) ) ;
#21487 = FACE_OUTER_BOUND ( 'NONE', #3443, .T. ) ;
#21488 = DIRECTION ( 'NONE',  ( -1.000000000000000000, 0.000000000000000000, 0.000000000000000000 ) ) ;
#21489 = EDGE_LOOP ( 'NONE', ( #23274, #8286, #14542, #23235 ) ) ;
#21490 = DIRECTION ( 'NONE',  ( 0.000000000000000000, 0.000000000000000000, 1.000000000000000000 ) ) ;
#21491 = ORIENTED_EDGE ( 'NONE', *, *, #19254, .T. ) ;
#21492 = SHAPE_REPRESENTATION_RELATIONSHIP ( 'NONE' , 'NONE' ,  #6919, #16897 ) ;
#21493 = ORIENTED_EDGE ( 'NONE', *, *, #1770, .F. ) ;
#21494 = VECTOR ( 'NONE', #4562, 1000.000000000000000 ) ;
#21495 = CARTESIAN_POINT ( 'NONE',  ( -38.39535039420000118, 26.50000000000000000, -147.5552959529999839 ) ) ;
#21496 = CARTESIAN_POINT ( 'NONE',  ( 32.50000000000000000, 32.96379895120000469, -137.0552959530000123 ) ) ;
#21497 = VERTEX_POINT ( 'NONE', #2666 ) ;
#21498 = CARTESIAN_POINT ( 'NONE',  ( 8.900000000049999471, 37.00000000000000000, -149.5552959529999839 ) ) ;
#21499 = VERTEX_POINT ( 'NONE', #17170 ) ;
#21500 = CARTESIAN_POINT ( 'NONE',  ( 24.01462304345166032, 39.11919234680899393, -136.0552959530542125 ) ) ;
#21501 = CARTESIAN_POINT ( 'NONE',  ( -20.34672008420000111, 36.01786665889999739, -139.8153362750000213 ) ) ;
#21502 = DIRECTION ( 'NONE',  ( 1.000000000000000000, 0.000000000000000000, -2.257157423930000049E-12 ) ) ;
#21503 = PLANE ( 'NONE',  #428 ) ;
#21504 = ORIENTED_EDGE ( 'NONE', *, *, #15053, .T. ) ;
#21505 = CARTESIAN_POINT ( 'NONE',  ( -7.041959465309999722, -26.08051538799999847, -142.5552959529999839 ) ) ;
#21506 = ORIENTED_EDGE ( 'NONE', *, *, #16152, .T. ) ;
#21507 = CARTESIAN_POINT ( 'NONE',  ( 9.371776569741914642, 35.77840329725038515, -141.8736084709495060 ) ) ;
#21508 = EDGE_CURVE ( 'NONE', #6588, #17682, #15502, .T. ) ;
#21509 = FACE_OUTER_BOUND ( 'NONE', #10970, .T. ) ;
#21510 = AXIS2_PLACEMENT_3D ( 'NONE', #2836, #10066, #17343 ) ;
#21511 = CARTESIAN_POINT ( 'NONE',  ( -32.50000000000000000, 69.41770215440000413, -140.5449657050000098 ) ) ;
#21512 = AXIS2_PLACEMENT_3D ( 'NONE', #5888, #20416, #16602 ) ;
#21513 = ORIENTED_EDGE ( 'NONE', *, *, #6162, .F. ) ;
#21514 = DIRECTION ( 'NONE',  ( 0.07970438983373200059, 0.9968185442904001770, -8.277822871613320832E-13 ) ) ;
#21515 = VERTEX_POINT ( 'NONE', #15385 ) ;
#21516 = CARTESIAN_POINT ( 'NONE',  ( -14.47770030809999930, -15.50000000000000000, -148.5552959529999839 ) ) ;
#21517 = CARTESIAN_POINT ( 'NONE',  ( -32.50000000000000000, 51.50000000000000000, -143.3052959529999839 ) ) ;
#21518 = ORIENTED_EDGE ( 'NONE', *, *, #11189, .F. ) ;
#21519 = CARTESIAN_POINT ( 'NONE',  ( -10.97748938910000049, 39.75689975739999937, -140.4868351200000234 ) ) ;
#21520 = ORIENTED_EDGE ( 'NONE', *, *, #21313, .F. ) ;
#21521 = CARTESIAN_POINT ( 'NONE',  ( -21.21916986615164902, 36.96385231546391736, -148.6710958206639646 ) ) ;
#21522 = DIRECTION ( 'NONE',  ( -2.508215857230000030E-12, 0.000000000000000000, 1.000000000000000000 ) ) ;
#21523 = ORIENTED_EDGE ( 'NONE', *, *, #10954, .F. ) ;
#21524 =( BOUNDED_CURVE ( )  B_SPLINE_CURVE ( 5, ( #10307, #22944, #8519, #23290, #3296, #5081 ),
 .UNSPECIFIED., .F., .F. ) 
 B_SPLINE_CURVE_WITH_KNOTS ( ( 6, 6 ),
 ( 0.000000000000000000, 1.570796326891506167 ),
 .UNSPECIFIED. ) 
 CURVE ( )  GEOMETRIC_REPRESENTATION_ITEM ( )  RATIONAL_B_SPLINE_CURVE ( ( 1.000000000000000000, 0.5999999999754248581, 0.3999999999754249025, 0.2999999999815686769, 0.2499999999877124679, 0.2500000000000000000 ) ) 
 REPRESENTATION_ITEM ( '' )  );
#21525 = EDGE_LOOP ( 'NONE', ( #15739, #7659, #892, #11436 ) ) ;
#21526 = CARTESIAN_POINT ( 'NONE',  ( -27.13569889285190229, 40.84437936193481988, -141.7271500514046920 ) ) ;
#21527 = VECTOR ( 'NONE', #7344, 1000.000000000000000 ) ;
#21528 = DIRECTION ( 'NONE',  ( -2.507771768020000122E-12, 0.000000000000000000, 1.000000000000000000 ) ) ;
#21529 = ORIENTED_EDGE ( 'NONE', *, *, #19443, .F. ) ;
#21530 = EDGE_CURVE ( 'NONE', #10763, #14413, #6337, .T. ) ;
#21531 = VECTOR ( 'NONE', #10009, 1000.000000000000000 ) ;
#21532 = DIRECTION ( 'NONE',  ( 2.506794771760000178E-12, 0.000000000000000000, -1.000000000000000000 ) ) ;
#21533 = PLANE ( 'NONE',  #13284 ) ;
#21534 = EDGE_CURVE ( 'NONE', #19480, #2516, #12160, .T. ) ;
#21535 = CARTESIAN_POINT ( 'NONE',  ( -12.50000000000000000, 22.50000000000000000, -150.0552959529999839 ) ) ;
#21536 = VERTEX_POINT ( 'NONE', #7995 ) ;
#21537 = DIRECTION ( 'NONE',  ( 1.000000000000000000, 0.000000000000000000, -2.258609965721802837E-12 ) ) ;
#21538 = ADVANCED_FACE ( 'NONE', ( #20745 ), #4560, .F. ) ;
#21539 = ORIENTED_EDGE ( 'NONE', *, *, #3157, .F. ) ;
#21540 = DIRECTION ( 'NONE',  ( 0.000000000000000000, 0.000000000000000000, 1.000000000000000000 ) ) ;
#21541 = DIRECTION ( 'NONE',  ( 0.2229045288590935092, 0.9748402797454081004, -3.928002761761645078E-13 ) ) ;
#21542 = CARTESIAN_POINT ( 'NONE',  ( -14.54684675599480137, 39.31632282492414276, -147.3469236774771502 ) ) ;
#21543 = CARTESIAN_POINT ( 'NONE',  ( -21.35824191589999899, -4.000000000000000000, -144.8157682190000060 ) ) ;
#21544 = AXIS2_PLACEMENT_3D ( 'NONE', #18079, #21422, #5108 ) ;
#21545 = ORIENTED_EDGE ( 'NONE', *, *, #17535, .F. ) ;
#21546 = CARTESIAN_POINT ( 'NONE',  ( -0.9520167400502704824, 19.51924065639803629, -136.0552959529979091 ) ) ;
#21547 = DIRECTION ( 'NONE',  ( -2.507771768019999718E-12, -1.592654864069999939E-17, 1.000000000000000000 ) ) ;
#21548 = DIRECTION ( 'NONE',  ( 0.4794255386042040601, 0.8775825618903723147, 0.000000000000000000 ) ) ;
#21549 = CARTESIAN_POINT ( 'NONE',  ( -32.50000000000000000, 14.00000000000000000, -144.0552959529999839 ) ) ;
#21550 = LINE ( 'NONE', #18209, #6136 ) ;
#21551 = LINE ( 'NONE', #16, #10571 ) ;
#21552 = EDGE_LOOP ( 'NONE', ( #2834, #4055, #20289, #23151, #6706, #1605, #12255, #8001 ) ) ;
#21553 = CARTESIAN_POINT ( 'NONE',  ( -0.7499999998430000314, 41.50000000000000000, -140.5552959529999839 ) ) ;
#21555 = DIRECTION ( 'NONE',  ( -1.000000000000000000, 0.000000000000000000, 2.245315044999999693E-12 ) ) ;
#21554 = B_SPLINE_CURVE_WITH_KNOTS ( 'NONE', 3,
 ( #6928, #15737, #12159, #10717 ),
 .UNSPECIFIED., .F., .F.,
 ( 4, 4 ),
 ( 0.000000000000000000, 1.000000000000000000 ),
 .UNSPECIFIED. ) ;
#21556 = CARTESIAN_POINT ( 'NONE',  ( 6.010856941112707297, -6.121359165062768781, -150.0552959529999839 ) ) ;
#21557 = CARTESIAN_POINT ( 'NONE',  ( -6.837524392801337392, 37.99761324335693757, -148.5285986741252771 ) ) ;
#21558 = CARTESIAN_POINT ( 'NONE',  ( -24.01715389780000010, 40.57582142210000598, -141.9832779239999923 ) ) ;
#21559 = DIRECTION ( 'NONE',  ( -1.000000000000000000, 0.000000000000000000, 0.000000000000000000 ) ) ;
#21560 = VECTOR ( 'NONE', #4912, 1000.000000000000000 ) ;
#21561 = ORIENTED_EDGE ( 'NONE', *, *, #2941, .F. ) ;
#21562 = EDGE_CURVE ( 'NONE', #20932, #12200, #21649, .T. ) ;
#21563 = CARTESIAN_POINT ( 'NONE',  ( -4.192924954330000453, -28.60725908990000121, -146.5552959529999839 ) ) ;
#21564 = CONICAL_SURFACE ( 'NONE', #17366, 1.999999999999992450, 0.7853981633970000820 ) ;
#21565 = DIRECTION ( 'NONE',  ( 8.955190032050000935E-12, -9.104778821549999739E-13, 1.000000000000000000 ) ) ;
#21566 = EDGE_CURVE ( 'NONE', #10756, #14446, #1134, .T. ) ;
#21567 = ORIENTED_EDGE ( 'NONE', *, *, #22668, .F. ) ;
#21568 = PRODUCT ( 'Latch Return Spring', 'Latch Return Spring', '', ( #14957 ) ) ;
#21569 = DIRECTION ( 'NONE',  ( 4.430318231639999944E-12, -6.100259101500000139E-13, 1.000000000000000000 ) ) ;
#21570 = ORIENTED_EDGE ( 'NONE', *, *, #1669, .T. ) ;
#21571 = CARTESIAN_POINT ( 'NONE',  ( -24.38851193153152508, 40.21356925245557790, -145.9141185447818998 ) ) ;
#21572 = CARTESIAN_POINT ( 'NONE',  ( -29.89717128122237000, 39.22683608722478965, -140.1129597738056418 ) ) ;
#21573 = DIRECTION ( 'NONE',  ( -1.000000000000000000, 0.000000000000000000, 0.000000000000000000 ) ) ;
#21574 = CARTESIAN_POINT ( 'NONE',  ( 8.037995166842678785, 38.42729146114034933, -142.0027968016258342 ) ) ;
#21575 = ORIENTED_EDGE ( 'NONE', *, *, #19734, .T. ) ;
#21576 = CARTESIAN_POINT ( 'NONE',  ( -10.69040905424370003, 35.19607541363222225, -139.6909101219067963 ) ) ;
#21577 = CARTESIAN_POINT ( 'NONE',  ( -1.000000000000000000, 20.50000000000000000, -150.0552959529999839 ) ) ;
#21578 = CIRCLE ( 'NONE', #12428, 0.4999999999999987788 ) ;
#21579 = CARTESIAN_POINT ( 'NONE',  ( -8.631906738831403914, 39.33441879577958389, -147.3392595813083119 ) ) ;
#21580 = CARTESIAN_POINT ( 'NONE',  ( -46.00000000000000000, 37.00000000000000000, -149.0552959529999839 ) ) ;
#21581 = ORIENTED_EDGE ( 'NONE', *, *, #3145, .T. ) ;
#21582 = AXIS2_PLACEMENT_3D ( 'NONE', #16822, #6225, #9771 ) ;
#21583 = DIRECTION ( 'NONE',  ( -1.000000000000000000, 0.000000000000000000, -2.506439500389999993E-12 ) ) ;
#21584 = EDGE_CURVE ( 'NONE', #5749, #1015, #4680, .T. ) ;
#21585 = ORIENTED_EDGE ( 'NONE', *, *, #18138, .T. ) ;
#21586 = CARTESIAN_POINT ( 'NONE',  ( -8.514310886093261033, 36.94123471669811209, -140.1199228270031938 ) ) ;
#21587 = CARTESIAN_POINT ( 'NONE',  ( -9.434278515689999978, -18.41834002140000237, -146.5552959529999839 ) ) ;
#21588 = CARTESIAN_POINT ( 'NONE',  ( -4.499932713002730900, 22.10251055751376015, -136.0552959529898374 ) ) ;
#21589 = VERTEX_POINT ( 'NONE', #2898 ) ;
#21590 = DIRECTION ( 'NONE',  ( -1.000000000000000000, 0.000000000000000000, 0.000000000000000000 ) ) ;
#21591 = DIRECTION ( 'NONE',  ( 2.257242012349999735E-12, 0.000000000000000000, 1.000000000000000000 ) ) ;
#21592 = EDGE_CURVE ( 'NONE', #10616, #8910, #18658, .T. ) ;
#21593 = EDGE_LOOP ( 'NONE', ( #1299, #3559, #14567, #3055 ) ) ;
#21594 = CARTESIAN_POINT ( 'NONE',  ( 19.00000000000000000, 39.50000000000000000, -136.0552959530000123 ) ) ;
#21595 = CIRCLE ( 'NONE', #20072, 14.99999999999999822 ) ;
#21596 = CARTESIAN_POINT ( 'NONE',  ( 18.98502865237968606, 25.11890206003841541, -150.0552959529999839 ) ) ;
#21597 = CARTESIAN_POINT ( 'NONE',  ( -2.499999999859999988, 20.50000000000000000, -147.5552959529999839 ) ) ;
#21598 = CARTESIAN_POINT ( 'NONE',  ( 23.19105773460000108, -15.44374190390000123, -146.0552959529999839 ) ) ;
#21599 = DIRECTION ( 'NONE',  ( 2.257144641397284947E-12, -2.714724913984255017E-24, 1.000000000000000000 ) ) ;
#21600 = EDGE_CURVE ( 'NONE', #12372, #3522, #12896, .T. ) ;
#21601 = PLANE ( 'NONE',  #4834 ) ;
#21602 = SHAPE_DEFINITION_REPRESENTATION ( #3785, #13440 ) ;
#21603 = DIRECTION ( 'NONE',  ( 0.7633862853691872896, 0.6459422414660880296, -5.370703881624201706E-14 ) ) ;
#21604 = DIRECTION ( 'NONE',  ( 2.839308199620000013E-14, 3.568879590630000244E-13, 1.000000000000000000 ) ) ;
#21605 = CARTESIAN_POINT ( 'NONE',  ( 14.00000000000000000, 20.50000000000000000, -151.0552959529999839 ) ) ;
#21606 = ORIENTED_EDGE ( 'NONE', *, *, #2549, .T. ) ;
#21607 = UNCERTAINTY_MEASURE_WITH_UNIT (LENGTH_MEASURE( 1.000000000000000082E-05 ), #3633, 'distance_accuracy_value', 'NONE');
#21608 = ORIENTED_EDGE ( 'NONE', *, *, #4674, .T. ) ;
#21609 =( NAMED_UNIT ( * ) SI_UNIT ( $, .STERADIAN. ) SOLID_ANGLE_UNIT ( ) );
#21610 = EDGE_CURVE ( 'NONE', #7733, #23343, #16447, .T. ) ;
#21611 = ADVANCED_FACE ( 'NONE', ( #11419 ), #3835, .T. ) ;
#21612 = VECTOR ( 'NONE', #22921, 1000.000000000000000 ) ;
#21613 = VERTEX_POINT ( 'NONE', #9629 ) ;
#21614 = CARTESIAN_POINT ( 'NONE',  ( -4.499999999949999996, 40.00000000000000000, -150.0552959529999839 ) ) ;
#21615 = DIRECTION ( 'NONE',  ( -0.000000000000000000, 1.000000000000000000, 0.000000000000000000 ) ) ;
#21616 = DIRECTION ( 'NONE',  ( 0.000000000000000000, 1.000000000000000000, 0.000000000000000000 ) ) ;
#21617 = CARTESIAN_POINT ( 'NONE',  ( -25.35824191589811960, -1.500000000000000000, -146.3157682190081630 ) ) ;
#21618 = EDGE_CURVE ( 'NONE', #22236, #10363, #10605, .T. ) ;
#21619 = ORIENTED_EDGE ( 'NONE', *, *, #8288, .F. ) ;
#21620 = DIRECTION ( 'NONE',  ( -2.257144641399999941E-12, 0.000000000000000000, -1.000000000000000000 ) ) ;
#21621 = ADVANCED_FACE ( 'NONE', ( #14656 ), #21926, .F. ) ;
#21622 = CARTESIAN_POINT ( 'NONE',  ( -6.320468577110000652, -16.70961797440000041, -146.5552959529999839 ) ) ;
#21623 = CARTESIAN_POINT ( 'NONE',  ( -12.28014746100000032, 36.97113097969999984, -148.4919582129999753 ) ) ;
#21624 = CARTESIAN_POINT ( 'NONE',  ( 22.00000000000000000, -20.50000000000000000, -137.2152959530000089 ) ) ;
#21625 = ORIENTED_EDGE ( 'NONE', *, *, #8768, .T. ) ;
#21626 = CARTESIAN_POINT ( 'NONE',  ( -15.46250806109999942, -1.500000000000000000, -147.7289441310000200 ) ) ;
#21627 = VERTEX_POINT ( 'NONE', #263 ) ;
#21628 = CARTESIAN_POINT ( 'NONE',  ( 9.863231070447312732, 36.37411343960744148, -141.6348998444321410 ) ) ;
#21629 = CARTESIAN_POINT ( 'NONE',  ( -2.499999999949999996, 42.50000000000000000, -150.0552959529999839 ) ) ;
#21630 = VECTOR ( 'NONE', #5616, 1000.000000000000000 ) ;
#21631 = DIRECTION ( 'NONE',  ( -2.508215857230000030E-12, 0.000000000000000000, 1.000000000000000000 ) ) ;
#21632 = ORIENTED_EDGE ( 'NONE', *, *, #21186, .F. ) ;
#21633 = VECTOR ( 'NONE', #22367, 999.9999999999998863 ) ;
#21634 = VECTOR ( 'NONE', #9274, 1000.000000000000000 ) ;
#21635 = DIRECTION ( 'NONE',  ( 0.000000000000000000, 0.000000000000000000, 1.000000000000000000 ) ) ;
#21636 = ORIENTED_EDGE ( 'NONE', *, *, #7490, .T. ) ;
#21637 = DIRECTION ( 'NONE',  ( -1.000000000000000000, 0.000000000000000000, 2.262368070660000099E-12 ) ) ;
#21638 = DIRECTION ( 'NONE',  ( 2.602084747549999882E-17, -1.000000000000000000, -5.873289694040000105E-29 ) ) ;
#21639 = ORIENTED_EDGE ( 'NONE', *, *, #20164, .T. ) ;
#21640 = LINE ( 'NONE', #19850, #17563 ) ;
#21641 = EDGE_CURVE ( 'NONE', #12270, #1424, #14772, .T. ) ;
#21642 = ORIENTED_EDGE ( 'NONE', *, *, #16367, .T. ) ;
#21643 = EDGE_CURVE ( 'NONE', #12394, #7397, #20259, .T. ) ;
#21644 = CARTESIAN_POINT ( 'NONE',  ( -3.765209112811370051, 42.50000000000000711, -150.0552959530000123 ) ) ;
#21645 = VERTEX_POINT ( 'NONE', #8442 ) ;
#21646 = CIRCLE ( 'NONE', #353, 8.176568160360000448 ) ;
#21647 = ORIENTED_EDGE ( 'NONE', *, *, #14171, .T. ) ;
#21648 = DIRECTION ( 'NONE',  ( 0.000000000000000000, 1.000000000000000000, 0.000000000000000000 ) ) ;
#21649 = CIRCLE ( 'NONE', #11348, 0.5000000000000004441 ) ;
#21650 = CARTESIAN_POINT ( 'NONE',  ( -10.41700570847820195, 37.07221587398770879, -140.3414633426674243 ) ) ;
#21651 = ORIENTED_EDGE ( 'NONE', *, *, #20826, .F. ) ;
#21652 = CARTESIAN_POINT ( 'NONE',  ( 0.3832000607639999834, -24.50000000000000000, -150.0552959529999839 ) ) ;
#21653 = VECTOR ( 'NONE', #4746, 1000.000000000000000 ) ;
#21654 = CARTESIAN_POINT ( 'NONE',  ( -18.35824191589999899, -1.500000000000000000, -150.0657682190000060 ) ) ;
#21655 = AXIS2_PLACEMENT_3D ( 'NONE', #5024, #23108, #17747 ) ;
#21656 = CARTESIAN_POINT ( 'NONE',  ( -29.18315392570000100, -50.50000000000000000, -137.0552959530000123 ) ) ;
#21657 = AXIS2_PLACEMENT_3D ( 'NONE', #2974, #17128, #15455 ) ;
#21658 = EDGE_LOOP ( 'NONE', ( #18986, #4243, #10817, #3208 ) ) ;
#21659 = LINE ( 'NONE', #1674, #3011 ) ;
#21660 = ORIENTED_EDGE ( 'NONE', *, *, #3997, .T. ) ;
#21661 = LINE ( 'NONE', #14272, #13166 ) ;
#21662 = VECTOR ( 'NONE', #14485, 1000.000000000000000 ) ;
#21663 = CARTESIAN_POINT ( 'NONE',  ( 15.59498359470000040, -26.23371093219999750, -148.0552959529999839 ) ) ;
#21664 =( REPRESENTATION_RELATIONSHIP ('NONE','NONE', #7672, #15746 ) REPRESENTATION_RELATIONSHIP_WITH_TRANSFORMATION ( #16244 )SHAPE_REPRESENTATION_RELATIONSHIP( ) );
#21665 = CARTESIAN_POINT ( 'NONE',  ( 6.500000000159999125, 20.50000000000000000, -140.5552959529999839 ) ) ;
#21666 = CARTESIAN_POINT ( 'NONE',  ( -28.33971964075230332, 37.08144121879533373, -140.0461821376590308 ) ) ;
#21667 = EDGE_LOOP ( 'NONE', ( #7119, #22194, #16159, #11221 ) ) ;
#21668 = FILL_AREA_STYLE ('',( #3573 ) ) ;
#21669 = CARTESIAN_POINT ( 'NONE',  ( -2.499999999859999988, 41.50000000000000000, -147.0552959529999839 ) ) ;
#21670 = VECTOR ( 'NONE', #1017, 1000.000000000000000 ) ;
#21671 =( BOUNDED_CURVE ( )  B_SPLINE_CURVE ( 5, ( #16761, #11735, #476, #7712, #14978, #22701 ),
 .UNSPECIFIED., .F., .F. ) 
 B_SPLINE_CURVE_WITH_KNOTS ( ( 6, 6 ),
 ( 0.000000000000000000, 1.570796326823717504 ),
 .UNSPECIFIED. ) 
 CURVE ( )  GEOMETRIC_REPRESENTATION_ITEM ( )  RATIONAL_B_SPLINE_CURVE ( ( 1.000000000000000000, 0.5999999999926871608, 0.3999999999926872052, 0.2999999999945154316, 0.2499999999963436192, 0.2500000000000000000 ) ) 
 REPRESENTATION_ITEM ( '' )  );
#21672 = AXIS2_PLACEMENT_3D ( 'NONE', #21237, #9785, #17185 ) ;
#21673 = CARTESIAN_POINT ( 'NONE',  ( 10.68320006080000084, -21.50000000000000000, -148.5552959529999839 ) ) ;
#21674 = FACE_OUTER_BOUND ( 'NONE', #17312, .T. ) ;
#21675 = LINE ( 'NONE', #10452, #9170 ) ;
#21676 = EDGE_CURVE ( 'NONE', #18387, #19018, #2635, .T. ) ;
#21677 = VECTOR ( 'NONE', #14872, 1000.000000000000000 ) ;
#21678 = FACE_OUTER_BOUND ( 'NONE', #6465, .T. ) ;
#21679 = AXIS2_PLACEMENT_3D ( 'NONE', #10552, #16170, #7120 ) ;
#21680 = VERTEX_POINT ( 'NONE', #15246 ) ;
#21681 = CARTESIAN_POINT ( 'NONE',  ( 6.000000000160000013, 32.99305018889999275, -140.5552959529999839 ) ) ;
#21682 = CARTESIAN_POINT ( 'NONE',  ( -13.69025052297850742, -42.24247369819922682, -136.0552959529691179 ) ) ;
#21683 = CARTESIAN_POINT ( 'NONE',  ( -32.50000000000000000, -51.50000000000000000, -142.8052959529999839 ) ) ;
#21684 = CARTESIAN_POINT ( 'NONE',  ( -5.064279449469999861, 40.47653686799999662, -142.0698957560000224 ) ) ;
#21685 = LINE ( 'NONE', #9029, #11938 ) ;
#21686 = EDGE_LOOP ( 'NONE', ( #5155, #13368, #12263, #8828 ) ) ;
#21687 = DIRECTION ( 'NONE',  ( 3.552713673710000046E-15, -1.000000000000000000, -8.018988631039999700E-27 ) ) ;
#21688 = DIRECTION ( 'NONE',  ( 1.000000000000000000, 0.000000000000000000, -8.955190032050000935E-12 ) ) ;
#21689 = ORIENTED_EDGE ( 'NONE', *, *, #9796, .F. ) ;
#21690 = VECTOR ( 'NONE', #23133, 1000.000000000000000 ) ;
#21691 = VECTOR ( 'NONE', #19597, 1000.000000000000000 ) ;
#21692 = CARTESIAN_POINT ( 'NONE',  ( 3.190056847791982175, -2.742569615067167010, -136.0552959530071746 ) ) ;
#21693 = ORIENTED_EDGE ( 'NONE', *, *, #11781, .F. ) ;
#21694 = PLANE ( 'NONE',  #9060 ) ;
#21695 = CARTESIAN_POINT ( 'NONE',  ( -29.80856694857513034, 37.96151168870303394, -140.1460686462327203 ) ) ;
#21696 = DIRECTION ( 'NONE',  ( -1.000000000000000000, 1.734728570689999873E-18, 2.257171095940000041E-12 ) ) ;
#21697 = CARTESIAN_POINT ( 'NONE',  ( 7.682970039224882086, 38.25799164440910971, -141.8948580842254614 ) ) ;
#21698 = ORIENTED_EDGE ( 'NONE', *, *, #2698, .T. ) ;
#21699 = CARTESIAN_POINT ( 'NONE',  ( -10.65913935279999869, 37.04331329920000115, -139.7140392919999954 ) ) ;
#21700 = CARTESIAN_POINT ( 'NONE',  ( -18.37691940378883970, 35.51168060186468267, -147.4900940510613907 ) ) ;
#21701 = EDGE_CURVE ( 'NONE', #13387, #14263, #4545, .T. ) ;
#21702 = CARTESIAN_POINT ( 'NONE',  ( -9.072898850179999641, 36.94639249900000522, -148.2684494029999769 ) ) ;
#21703 = LINE ( 'NONE', #17886, #13737 ) ;
#21704 = EDGE_CURVE ( 'NONE', #13141, #8311, #15710, .T. ) ;
#21705 = ORIENTED_EDGE ( 'NONE', *, *, #7410, .F. ) ;
#21706 = EDGE_CURVE ( 'NONE', #5909, #13263, #9982, .T. ) ;
#21707 = VECTOR ( 'NONE', #16116, 1000.000000000000000 ) ;
#21708 = DIRECTION ( 'NONE',  ( -2.257144641399999941E-12, 8.049635416090000264E-35, -1.000000000000000000 ) ) ;
#21709 = ORIENTED_EDGE ( 'NONE', *, *, #17610, .T. ) ;
#21710 = LINE ( 'NONE', #5395, #14898 ) ;
#21711 = CARTESIAN_POINT ( 'NONE',  ( -23.34997301940000014, 41.23575095009999814, -144.6233831890000090 ) ) ;
#21712 = DIRECTION ( 'NONE',  ( 0.000000000000000000, -1.000000000000000000, 0.000000000000000000 ) ) ;
#21713 = VERTEX_POINT ( 'NONE', #22613 ) ;
#21714 = DIRECTION ( 'NONE',  ( -0.2208456705930775810, -0.9753087663813413410, 1.089717887850382194E-12 ) ) ;
#21715 = DIRECTION ( 'NONE',  ( 1.000000000000000000, 0.000000000000000000, 2.516505522483685870E-12 ) ) ;
#21716 = ORIENTED_EDGE ( 'NONE', *, *, #21831, .T. ) ;
#21717 = CARTESIAN_POINT ( 'NONE',  ( -17.10091063390000343, 39.14571640540000175, -141.0837638240000160 ) ) ;
#21718 = CARTESIAN_POINT ( 'NONE',  ( 20.10234832539997285, 19.49999999999999645, -150.0552959530000123 ) ) ;
#21719 = DIRECTION ( 'NONE',  ( 0.000000000000000000, 1.000000000000000000, -2.245315044929999938E-12 ) ) ;
#21720 = VECTOR ( 'NONE', #12095, 1000.000000000000114 ) ;
#21721 = DIRECTION ( 'NONE',  ( -1.000000000000000000, 0.000000000000000000, 2.257076750570000197E-12 ) ) ;
#21722 = CIRCLE ( 'NONE', #14098, 3.000000000000000000 ) ;
#21723 = DIRECTION ( 'NONE',  ( 1.000000000000000000, 0.000000000000000000, -2.257120985840000117E-12 ) ) ;
#21724 = LINE ( 'NONE', #6953, #4070 ) ;
#21725 = ITEM_DEFINED_TRANSFORMATION ( 'NONE', 'NONE', #14943,  #5025 ) ;
#21726 = FACE_OUTER_BOUND ( 'NONE', #21729, .T. ) ;
#21727 = PLANE ( 'NONE',  #14268 ) ;
#21728 = FACE_OUTER_BOUND ( 'NONE', #13016, .T. ) ;
#21729 = EDGE_LOOP ( 'NONE', ( #20186, #15906, #1612, #7801 ) ) ;
#21730 = EDGE_CURVE ( 'NONE', #18905, #5196, #19042, .T. ) ;
#21731 = ORIENTED_EDGE ( 'NONE', *, *, #5268, .T. ) ;
#21732 =( NAMED_UNIT ( * ) SI_UNIT ( $, .STERADIAN. ) SOLID_ANGLE_UNIT ( ) );
#21733 = VERTEX_POINT ( 'NONE', #8196 ) ;
#21734 = CARTESIAN_POINT ( 'NONE',  ( 13.68320006080000084, -20.50000000000000000, -148.5552959529999839 ) ) ;
#21735 = CARTESIAN_POINT ( 'NONE',  ( -13.04270098951570134, 34.92521805816488012, -147.0831430690302000 ) ) ;
#21736 = DIRECTION ( 'NONE',  ( 1.526468026909999897E-13, 8.159623473500000156E-13, 1.000000000000000000 ) ) ;
#21737 = CARTESIAN_POINT ( 'NONE',  ( 13.95201674008816006, 21.48075934359548356, -136.0552959530315604 ) ) ;
#21738 = CIRCLE ( 'NONE', #14882, 8.176568160360000448 ) ;
#21739 = VERTEX_POINT ( 'NONE', #11646 ) ;
#21740 = CARTESIAN_POINT ( 'NONE',  ( 1.133692148650000009, 51.00000000000000000, -136.0552959530000123 ) ) ;
#21741 = ADVANCED_FACE ( 'NONE', ( #15468 ), #22972, .F. ) ;
#21742 = LINE ( 'NONE', #5430, #22812 ) ;
#21743 = CARTESIAN_POINT ( 'NONE',  ( -11.76216916721041805, 37.71582637476514321, -147.9848159988354723 ) ) ;
#21744 = CARTESIAN_POINT ( 'NONE',  ( 18.95053822279999878, 50.00000000000000000, -149.5552959529999839 ) ) ;
#21745 = ORIENTED_EDGE ( 'NONE', *, *, #676, .T. ) ;
#21746 = CARTESIAN_POINT ( 'NONE',  ( -13.86630785130000021, 50.50000000000000000, -136.5552959530000123 ) ) ;
#21747 = ORIENTED_EDGE ( 'NONE', *, *, #15416, .T. ) ;
#21748 = CARTESIAN_POINT ( 'NONE',  ( 8.711528040173069698, 35.51461027188803143, -142.0444128376234687 ) ) ;
#21749 = ADVANCED_FACE ( 'NONE', ( #9866 ), #12010, .T. ) ;
#21750 = CARTESIAN_POINT ( 'NONE',  ( -6.683153925719999222, 51.50000000000000000, -136.0552959530000123 ) ) ;
#21751 = DIRECTION ( 'NONE',  ( -1.000000000000000000, 0.000000000000000000, 2.258108725280000263E-12 ) ) ;
#21752 = STYLED_ITEM ( 'NONE', ( #8261 ), #3292 ) ;
#21753 = ORIENTED_EDGE ( 'NONE', *, *, #6126, .T. ) ;
#21754 = VECTOR ( 'NONE', #20405, 999.9999999999998863 ) ;
#21755 = ADVANCED_FACE ( 'NONE', ( #6657 ), #17140, .T. ) ;
#21756 = ADVANCED_FACE ( 'NONE', ( #4301 ), #20958, .F. ) ;
#21757 = CARTESIAN_POINT ( 'NONE',  ( 16.62554907222028078, -18.90013506635313334, -146.5552959530255350 ) ) ;
#21758 = ORIENTED_EDGE ( 'NONE', *, *, #23514, .T. ) ;
#21759 = CARTESIAN_POINT ( 'NONE',  ( -7.129475577410000042, -25.57825421080000083, -143.5552959529999839 ) ) ;
#21760 = PLANE ( 'NONE',  #1780 ) ;
#21761 = ORIENTED_EDGE ( 'NONE', *, *, #21530, .T. ) ;
#21762 = DIRECTION ( 'NONE',  ( -1.000000000000000000, 0.000000000000000000, 2.257144641399999941E-12 ) ) ;
#21763 = ORIENTED_EDGE ( 'NONE', *, *, #20092, .F. ) ;
#21764 = CARTESIAN_POINT ( 'NONE',  ( -15.67604317050167140, 40.52459757754237302, -145.9876088847360052 ) ) ;
#21765 = LINE ( 'NONE', #18179, #4513 ) ;
#21766 = VERTEX_POINT ( 'NONE', #13444 ) ;
#21767 = DIRECTION ( 'NONE',  ( 0.000000000000000000, 0.000000000000000000, 1.000000000000000000 ) ) ;
#21768 = ORIENTED_EDGE ( 'NONE', *, *, #6735, .F. ) ;
#21769 = CARTESIAN_POINT ( 'NONE',  ( -26.53689163751006674, 38.88307050151443889, -139.6803910534961517 ) ) ;
#21770 = EDGE_CURVE ( 'NONE', #9931, #3657, #20044, .T. ) ;
#21771 = CARTESIAN_POINT ( 'NONE',  ( 31.50000000000000000, -40.03620104880000241, -136.0552959530000123 ) ) ;
#21772 = EDGE_LOOP ( 'NONE', ( #21056, #15639, #21806, #21504 ) ) ;
#21773 =( GEOMETRIC_REPRESENTATION_CONTEXT ( 3 ) GLOBAL_UNCERTAINTY_ASSIGNED_CONTEXT ( ( #19471 ) ) GLOBAL_UNIT_ASSIGNED_CONTEXT ( ( #12419, #13983, #8852 ) ) REPRESENTATION_CONTEXT ( 'NONE', 'WORKASPACE' ) );
#21774 = LINE ( 'NONE', #12282, #10250 ) ;
#21775 = EDGE_CURVE ( 'NONE', #11995, #13663, #18807, .T. ) ;
#21776 = VECTOR ( 'NONE', #19509, 1000.000000000000114 ) ;
#21777 = LINE ( 'NONE', #10908, #32 ) ;
#21778 = PLANE ( 'NONE',  #6412 ) ;
#21779 = EDGE_LOOP ( 'NONE', ( #18324, #14008, #4018, #23041 ) ) ;
#21780 = EDGE_CURVE ( 'NONE', #19866, #18293, #1087, .T. ) ;
#21781 = DIRECTION ( 'NONE',  ( -0.7071067811865473507, -0.7071067811865476838, 1.591319668629389897E-12 ) ) ;
#21782 = ADVANCED_FACE ( 'NONE', ( #2757 ), #15595, .F. ) ;
#21783 = ORIENTED_EDGE ( 'NONE', *, *, #5060, .T. ) ;
#21784 = CARTESIAN_POINT ( 'NONE',  ( 31.50000000000000000, -33.03620104880000241, -137.0552959530000123 ) ) ;
#21785 = EDGE_CURVE ( 'NONE', #2980, #7907, #21076, .T. ) ;
#21786 = LINE ( 'NONE', #14390, #20720 ) ;
#21787 = CARTESIAN_POINT ( 'NONE',  ( -17.10091063381063847, 39.14571640549888087, -141.0837638240818137 ) ) ;
#21788 = CARTESIAN_POINT ( 'NONE',  ( -22.10875017890000294, 36.18377167419999552, -148.1739623899999856 ) ) ;
#21789 = ORIENTED_EDGE ( 'NONE', *, *, #6323, .F. ) ;
#21790 = CARTESIAN_POINT ( 'NONE',  ( 1.133692148650000009, -2.273736754430000208E-12, -136.0552959530000123 ) ) ;
#21791 = PLANE ( 'NONE',  #18844 ) ;
#21792 = CARTESIAN_POINT ( 'NONE',  ( 23.50000000000000000, -20.50000000000000000, -136.0552959530000123 ) ) ;
#21793 = CARTESIAN_POINT ( 'NONE',  ( -30.49999999990000177, 26.50000000000000000, -140.5552959529999839 ) ) ;
#21794 = LINE ( 'NONE', #10926, #16411 ) ;
#21795 = DIRECTION ( 'NONE',  ( 0.7633862853691522066, 0.6459422414661292189, 1.795096815436260566E-28 ) ) ;
#21796 = ORIENTED_EDGE ( 'NONE', *, *, #21730, .T. ) ;
#21797 = SURFACE_STYLE_FILL_AREA ( #23214 ) ;
#21798 = PLANE ( 'NONE',  #14457 ) ;
#21799 = FACE_OUTER_BOUND ( 'NONE', #13865, .T. ) ;
#21800 = CARTESIAN_POINT ( 'NONE',  ( -5.537589236589999686, 40.52957482200000072, -146.1175057039999956 ) ) ;
#21801 = DIRECTION ( 'NONE',  ( 1.000000000000000000, 0.000000000000000000, 0.000000000000000000 ) ) ;
#21802 = EDGE_LOOP ( 'NONE', ( #4520, #2267, #7772, #19309 ) ) ;
#21803 = DIRECTION ( 'NONE',  ( -8.955058916629999092E-12, 9.112710586119999183E-13, -1.000000000000000000 ) ) ;
#21804 = DIRECTION ( 'NONE',  ( 0.000000000000000000, 1.000000000000000000, -2.245315044929999938E-12 ) ) ;
#21805 = LINE ( 'NONE', #18183, #16702 ) ;
#21806 = ORIENTED_EDGE ( 'NONE', *, *, #16339, .F. ) ;
#21807 = EDGE_CURVE ( 'NONE', #350, #15992, #17492, .T. ) ;
#21808 = EDGE_CURVE ( 'NONE', #20679, #10162, #15177, .T. ) ;
#21809 = FACE_OUTER_BOUND ( 'NONE', #3276, .T. ) ;
#21810 = VERTEX_POINT ( 'NONE', #7012 ) ;
#21811 =( BOUNDED_SURFACE ( )  B_SPLINE_SURFACE ( 5, 5, ( 
 ( #8115, #8475, #20636, #11565, #18840, #17407 ),
 ( #2788, #4683, #8233, #17049, #20868, #2548 ),
 ( #22536, #767, #15388, #8000, #6227, #10014 ),
 ( #15281, #22765, #6463, #11925, #19191, #13476 ),
 ( #20749, #4443, #11679, #891, #18956, #9896 ),
 ( #22647, #10480, #19553, #8936, #23003, #18118 ),
 ( #9045, #16216, #14307, #8822, #10722, #4917 ),
 ( #18003, #21225, #1356, #8581, #3487, #1714 ),
 ( #1476, #21579, #15855, #12511, #5260, #23120 ),
 ( #17885, #10371, #17647, #19907, #3605, #14430 ),
 ( #12636, #19793, #10835, #21459, #23469, #7164 ),
 ( #21702, #16099, #5389, #12165, #3141, #1829 ) ),
 .UNSPECIFIED., .F., .F., .F. ) 
 B_SPLINE_SURFACE_WITH_KNOTS ( ( 6, 3, 3, 6 ),
 ( 6, 6 ),
 ( 0.000000000000000000, 4.371092480729999785, 8.745625541600000830, 13.12578902609999965 ),
 ( 0.000000000000000000, 1.570796326891464867 ),
 .UNSPECIFIED. ) 
 GEOMETRIC_REPRESENTATION_ITEM ( )  RATIONAL_B_SPLINE_SURFACE ( (
 ( 1.000000000000000000, 0.5999999999754349611, 0.3999999999754355051, 0.2999999999815765039, 0.2499999999877174917, 0.2500000000000000000),
 ( 1.000000000000000000, 0.5999999999754349611, 0.3999999999754355051, 0.2999999999815765039, 0.2499999999877174917, 0.2500000000000000000),
 ( 1.000000000000000000, 0.5999999999754349611, 0.3999999999754355051, 0.2999999999815765039, 0.2499999999877174917, 0.2500000000000000000),
 ( 1.000000000000000000, 0.5999999999754349611, 0.3999999999754355051, 0.2999999999815765039, 0.2499999999877174917, 0.2500000000000000000),
 ( 1.000000000000000000, 0.5999999999754349611, 0.3999999999754355051, 0.2999999999815765039, 0.2499999999877174917, 0.2500000000000000000),
 ( 1.000000000000000000, 0.5999999999754349611, 0.3999999999754355051, 0.2999999999815765039, 0.2499999999877174917, 0.2500000000000000000),
 ( 1.000000000000000000, 0.5999999999754349611, 0.3999999999754355051, 0.2999999999815765039, 0.2499999999877174917, 0.2500000000000000000),
 ( 1.000000000000000000, 0.5999999999754349611, 0.3999999999754355051, 0.2999999999815765039, 0.2499999999877174917, 0.2500000000000000000),
 ( 1.000000000000000000, 0.5999999999754349611, 0.3999999999754355051, 0.2999999999815765039, 0.2499999999877174917, 0.2500000000000000000),
 ( 1.000000000000000000, 0.5999999999754349611, 0.3999999999754355051, 0.2999999999815765039, 0.2499999999877174917, 0.2500000000000000000),
 ( 1.000000000000000000, 0.5999999999754349611, 0.3999999999754355051, 0.2999999999815765039, 0.2499999999877174917, 0.2500000000000000000),
 ( 1.000000000000000000, 0.5999999999754349611, 0.3999999999754355051, 0.2999999999815765039, 0.2499999999877174917, 0.2500000000000000000) ) ) 
 REPRESENTATION_ITEM ( '' )  SURFACE ( )  );
#21812 = CYLINDRICAL_SURFACE ( 'NONE', #18961, 7.000000000000000888 ) ;
#21813 = CARTESIAN_POINT ( 'NONE',  ( 1.133692148550000001, 50.50000000000000000, -136.0552959530000123 ) ) ;
#21814 = DIRECTION ( 'NONE',  ( 1.000000000000000000, 0.000000000000000000, -2.259525899719999991E-12 ) ) ;
#21815 = CARTESIAN_POINT ( 'NONE',  ( 7.922905632975483670, 38.38455376863645085, -141.9737733526858960 ) ) ;
#21816 = ORIENTED_EDGE ( 'NONE', *, *, #13915, .T. ) ;
#21817 = CARTESIAN_POINT ( 'NONE',  ( -11.17931034166987203, 33.41890892721424677, -141.8539557988947877 ) ) ;
#21818 = CARTESIAN_POINT ( 'NONE',  ( -19.82031220496693180, 35.98978369854768289, -139.3867682255206262 ) ) ;
#21819 = PLANE ( 'NONE',  #13213 ) ;
#21820 = CARTESIAN_POINT ( 'NONE',  ( 4.204281436816111217, -32.13417682219588301, -136.0552959530095052 ) ) ;
#21821 = VERTEX_POINT ( 'NONE', #14039 ) ;
#21822 = CARTESIAN_POINT ( 'NONE',  ( -12.50000000000000000, 19.50000000000000000, -151.0552959529999839 ) ) ;
#21823 = ORIENTED_EDGE ( 'NONE', *, *, #905, .F. ) ;
#21824 = DIRECTION ( 'NONE',  ( 2.839308199620000013E-14, 3.568879590630000244E-13, 1.000000000000000000 ) ) ;
#21825 = CARTESIAN_POINT ( 'NONE',  ( 24.85988213910000155, -26.16224997189999968, -145.5552959529999839 ) ) ;
#21826 = CARTESIAN_POINT ( 'NONE',  ( -4.880807653152064773, 20.98537695657578084, -136.0552959529889847 ) ) ;
#21827 = ORIENTED_EDGE ( 'NONE', *, *, #20971, .F. ) ;
#21828 = PLANE ( 'NONE',  #9860 ) ;
#21829 = DIRECTION ( 'NONE',  ( 5.094701932209999624E-24, 1.000000000000000000, -1.149947916579999802E-35 ) ) ;
#21830 = ORIENTED_EDGE ( 'NONE', *, *, #4003, .T. ) ;
#21831 = EDGE_CURVE ( 'NONE', #844, #21875, #12125, .T. ) ;
#21832 = CARTESIAN_POINT ( 'NONE',  ( 23.21181482502162297, -23.48612613680712968, -142.5552959529975112 ) ) ;
#21833 = EDGE_CURVE ( 'NONE', #4750, #8854, #6816, .T. ) ;
#21834 = DIRECTION ( 'NONE',  ( -1.000000000000000000, 0.000000000000000000, 2.257144641399999941E-12 ) ) ;
#21835 = CARTESIAN_POINT ( 'NONE',  ( 8.500000000050000892, 37.00000000000000000, -149.5552959529999839 ) ) ;
#21836 = EDGE_CURVE ( 'NONE', #6188, #10194, #14810, .T. ) ;
#21837 = CARTESIAN_POINT ( 'NONE',  ( -24.63187620837634739, 37.01311550627328018, -148.7335123084583302 ) ) ;
#21838 = DIRECTION ( 'NONE',  ( 1.000000000000000000, -5.094701932209999624E-24, 0.000000000000000000 ) ) ;
#21839 = AXIS2_PLACEMENT_3D ( 'NONE', #14206, #1257, #1483 ) ;
#21840 = CARTESIAN_POINT ( 'NONE',  ( 15.50000000000000000, 39.50000000000000000, -150.0552959529999839 ) ) ;
#21841 = APPLICATION_PROTOCOL_DEFINITION ( 'draft international standard', 'automotive_design', 1998, #9462 ) ;
#21842 = DIRECTION ( 'NONE',  ( 0.000000000000000000, 1.000000000000000000, 0.000000000000000000 ) ) ;
#21843 = DIRECTION ( 'NONE',  ( -3.994014902950000436E-29, 1.000000000000000000, -4.148443855749999753E-27 ) ) ;
#21844 = PRODUCT_DEFINITION_SHAPE ( 'NONE', 'NONE',  #11950 ) ;
#21845 = CARTESIAN_POINT ( 'NONE',  ( -31.50000000000000000, -24.50000000000000000, -150.0552959529999839 ) ) ;
#21846 = ORIENTED_EDGE ( 'NONE', *, *, #18534, .F. ) ;
#21847 = UNCERTAINTY_MEASURE_WITH_UNIT (LENGTH_MEASURE( 1.000000000000000082E-05 ), #15219, 'distance_accuracy_value', 'NONE');
#21848 = ORIENTED_EDGE ( 'NONE', *, *, #1837, .F. ) ;
#21849 = FILL_AREA_STYLE ('',( #20180 ) ) ;
#21850 = ORIENTED_EDGE ( 'NONE', *, *, #20534, .F. ) ;
#21851 = CARTESIAN_POINT ( 'NONE',  ( -16.90886450125455198, 35.01031021513652775, -141.1892970147640085 ) ) ;
#21852 = PLANE ( 'NONE',  #21346 ) ;
#21853 = ORIENTED_EDGE ( 'NONE', *, *, #16797, .T. ) ;
#21854 = CARTESIAN_POINT ( 'NONE',  ( -18.18930989820000121, 36.96028804430000037, -147.6841622079999752 ) ) ;
#21855 = ORIENTED_EDGE ( 'NONE', *, *, #5242, .T. ) ;
#21856 = CARTESIAN_POINT ( 'NONE',  ( -5.098088255175412087, 24.33948587670916908, -150.0552959529999839 ) ) ;
#21857 = CARTESIAN_POINT ( 'NONE',  ( -19.49544947696901787, 34.86113041125985745, -141.2543152433912041 ) ) ;
#21858 = PLANE ( 'NONE',  #20466 ) ;
#21859 = ORIENTED_EDGE ( 'NONE', *, *, #8509, .F. ) ;
#21860 = CYLINDRICAL_SURFACE ( 'NONE', #20931, 2.000000000000001776 ) ;
#21861 = EDGE_CURVE ( 'NONE', #18962, #6192, #16301, .T. ) ;
#21862 = ORIENTED_EDGE ( 'NONE', *, *, #4333, .T. ) ;
#21863 = CARTESIAN_POINT ( 'NONE',  ( 9.334143923700091605, 35.75332166666289879, -141.8883195129358228 ) ) ;
#21864 = EDGE_CURVE ( 'NONE', #8311, #15451, #15943, .T. ) ;
#21865 = LINE ( 'NONE', #9223, #16557 ) ;
#21866 = DIRECTION ( 'NONE',  ( 0.7633862853691524286, -0.6459422414661292189, 2.747801985950550015E-15 ) ) ;
#21867 = ORIENTED_EDGE ( 'NONE', *, *, #19817, .F. ) ;
#21868 = EDGE_CURVE ( 'NONE', #12270, #2516, #18083, .T. ) ;
#21869 = DIRECTION ( 'NONE',  ( 0.000000000000000000, 0.000000000000000000, 1.000000000000000000 ) ) ;
#21870 = ORIENTED_EDGE ( 'NONE', *, *, #23457, .T. ) ;
#21871 = CIRCLE ( 'NONE', #4753, 5.000000000000000000 ) ;
#21872 = DIRECTION ( 'NONE',  ( 0.6427876096872939815, 0.000000000000000000, 0.7660444431183448533 ) ) ;
#21873 = VERTEX_POINT ( 'NONE', #21194 ) ;
#21874 = CARTESIAN_POINT ( 'NONE',  ( -6.320468577110000652, -16.70961797440000041, -147.5552959529999839 ) ) ;
#21875 = VERTEX_POINT ( 'NONE', #8785 ) ;
#21876 = CARTESIAN_POINT ( 'NONE',  ( -22.36496694526604756, 35.22036549038422493, -139.8269661872139409 ) ) ;
#21877 = CARTESIAN_POINT ( 'NONE',  ( 6.959824834146532524, -28.67531053199257229, -145.5552959530214991 ) ) ;
#21878 = ORIENTED_EDGE ( 'NONE', *, *, #20315, .T. ) ;
#21879 = APPLICATION_PROTOCOL_DEFINITION ( 'draft international standard', 'automotive_design', 1998, #7051 ) ;
#21880 = EDGE_CURVE ( 'NONE', #7890, #3203, #6774, .T. ) ;
#21881 = ORIENTED_EDGE ( 'NONE', *, *, #2124, .F. ) ;
#21882 = CARTESIAN_POINT ( 'NONE',  ( -26.33255611194164558, 36.96293009473756541, -139.4434112040622153 ) ) ;
#21883 = CARTESIAN_POINT ( 'NONE',  ( 27.18320006080000084, 3.500000000000000000, -150.0552959529999839 ) ) ;
#21884 = CARTESIAN_POINT ( 'NONE',  ( 23.50000000000000000, -20.50000000000000000, -137.0552959530000123 ) ) ;
#21885 = DIRECTION ( 'NONE',  ( 1.000000000000000000, 0.000000000000000000, -4.430318231639999944E-12 ) ) ;
#21886 = PLANE ( 'NONE',  #22759 ) ;
#21887 = EDGE_LOOP ( 'NONE', ( #11716, #15890, #10138, #7042 ) ) ;
#21888 = DIRECTION ( 'NONE',  ( 2.257305453670000045E-12, 0.000000000000000000, 1.000000000000000000 ) ) ;
#21889 = AXIS2_PLACEMENT_3D ( 'NONE', #67, #22070, #5636 ) ;
#21890 = EDGE_CURVE ( 'NONE', #1427, #7689, #17725, .T. ) ;
#21891 = VECTOR ( 'NONE', #1624, 1000.000000000000227 ) ;
#21892 = DIRECTION ( 'NONE',  ( -0.1435602414469281940, -0.9896415801065048257, 3.847089866708073804E-13 ) ) ;
#21893 = VERTEX_POINT ( 'NONE', #5111 ) ;
#21894 = CARTESIAN_POINT ( 'NONE',  ( -9.282104535860000283, -16.71402168319999859, -145.5552959529999839 ) ) ;
#21895 = DIRECTION ( 'NONE',  ( 1.000000000000000000, 0.000000000000000000, 0.000000000000000000 ) ) ;
#21896 = EDGE_CURVE ( 'NONE', #15683, #2935, #19631, .T. ) ;
#21897 = FACE_OUTER_BOUND ( 'NONE', #5329, .T. ) ;
#21898 = CARTESIAN_POINT ( 'NONE',  ( -23.02519999780000148, 33.35976406540000028, -141.9520978260000277 ) ) ;
#21899 = EDGE_LOOP ( 'NONE', ( #22102, #10551, #1964, #17432, #20350, #8772, #5463, #12494, #20960, #8548, #6947, #12172, #8761, #22401, #6939, #21041, #1158, #5487, #18191, #3547, #17124, #10564, #9694, #165, #20449, #4796, #7427, #8543, #5717, #17702, #20019, #19138 ) ) ;
#21900 = CARTESIAN_POINT ( 'NONE',  ( -15.61190926919999988, -34.50000000000000000, -146.8816477750000047 ) ) ;
#21901 = DIRECTION ( 'NONE',  ( 0.000000000000000000, 1.000000000000000000, 0.000000000000000000 ) ) ;
#21902 = FACE_BOUND ( 'NONE', #12204, .T. ) ;
#21903 = DIRECTION ( 'NONE',  ( 0.000000000000000000, 1.000000000000000000, 0.000000000000000000 ) ) ;
#21904 = DIRECTION ( 'NONE',  ( -2.507771768019999718E-12, -1.592654864069999939E-17, 1.000000000000000000 ) ) ;
#21905 = PLANE ( 'NONE',  #22368 ) ;
#21906 = AXIS2_PLACEMENT_3D ( 'NONE', #14010, #23176, #21403 ) ;
#21907 = VECTOR ( 'NONE', #22502, 1000.000000000000000 ) ;
#21908 = ORIENTED_EDGE ( 'NONE', *, *, #4224, .F. ) ;
#21909 = CARTESIAN_POINT ( 'NONE',  ( -27.44856507211657615, 33.04311423941999948, -146.2071622461182017 ) ) ;
#21910 = ADVANCED_FACE ( 'NONE', ( #1326 ), #23087, .F. ) ;
#21911 = CARTESIAN_POINT ( 'NONE',  ( -22.10824191589999899, -32.00000000000000000, -146.2257682199999920 ) ) ;
#21912 = CARTESIAN_POINT ( 'NONE',  ( 2.989143058887309135, -6.121359165062779439, -150.0552959529999839 ) ) ;
#21913 = ADVANCED_FACE ( 'NONE', ( #12244 ), #3595, .F. ) ;
#21914 = CARTESIAN_POINT ( 'NONE',  ( -5.385270659705732044, 41.64123329751902958, -144.5533759557629310 ) ) ;
#21915 = CARTESIAN_POINT ( 'NONE',  ( 2.499999999879999990, -3.000000000000000000, -135.4552959529999896 ) ) ;
#21916 = EDGE_CURVE ( 'NONE', #4825, #3746, #2035, .T. ) ;
#21917 = VERTEX_POINT ( 'NONE', #16637 ) ;
#21918 = LINE ( 'NONE', #144, #21634 ) ;
#21919 = EDGE_CURVE ( 'NONE', #12787, #6002, #9139, .T. ) ;
#21920 = CARTESIAN_POINT ( 'NONE',  ( 3.000000000000000888, -3.300910577262573309, -150.0552959529999839 ) ) ;
#21921 = ORIENTED_EDGE ( 'NONE', *, *, #3184, .F. ) ;
#21922 = AXIS2_PLACEMENT_3D ( 'NONE', #21597, #10740, #19923 ) ;
#21923 = ORIENTED_EDGE ( 'NONE', *, *, #9526, .T. ) ;
#21924 = CARTESIAN_POINT ( 'NONE',  ( -22.60318121862521323, 35.64391590581870162, -140.8717365814055995 ) ) ;
#21925 = DIRECTION ( 'NONE',  ( 2.257083409060000051E-12, 0.000000000000000000, 1.000000000000000000 ) ) ;
#21926 = PLANE ( 'NONE',  #17071 ) ;
#21927 = VERTEX_POINT ( 'NONE', #12953 ) ;
#21928 = CARTESIAN_POINT ( 'NONE',  ( -11.40196181638443207, 35.19900947717987805, -139.9192633046721994 ) ) ;
#21929 = CARTESIAN_POINT ( 'NONE',  ( -18.46643761655235849, 34.84883242740267661, -147.1252693406791821 ) ) ;
#21930 = FACE_OUTER_BOUND ( 'NONE', #22596, .T. ) ;
#21931 = CARTESIAN_POINT ( 'NONE',  ( 15.50000000000000000, 33.50000000000000000, -136.0552959530000123 ) ) ;
#21932 = DIRECTION ( 'NONE',  ( -2.257144641399999941E-12, 0.000000000000000000, 1.000000000000000000 ) ) ;
#21933 = CARTESIAN_POINT ( 'NONE',  ( 18.98537695664905556, 19.88080765317965870, -136.0552959530428438 ) ) ;
#21934 = CIRCLE ( 'NONE', #2934, 0.7500000000000006661 ) ;
#21935 = ADVANCED_FACE ( 'NONE', ( #16876 ), #14866, .T. ) ;
#21936 = VECTOR ( 'NONE', #2140, 1000.000000000000000 ) ;
#21937 = PLANE ( 'NONE',  #5405 ) ;
#21938 = DIRECTION ( 'NONE',  ( 2.257749542879999954E-12, 0.000000000000000000, 1.000000000000000000 ) ) ;
#21939 = CARTESIAN_POINT ( 'NONE',  ( -9.347107914279998653, -17.32706600430000066, -144.5552959529999839 ) ) ;
#21940 = EDGE_LOOP ( 'NONE', ( #3850, #13204, #12579, #13695 ) ) ;
#21941 = CARTESIAN_POINT ( 'NONE',  ( -5.366752052302948606, 40.61197287204888084, -143.6738006028257928 ) ) ;
#21942 = ORIENTED_EDGE ( 'NONE', *, *, #2416, .F. ) ;
#21943 =( BOUNDED_SURFACE ( )  B_SPLINE_SURFACE ( 5, 5, ( 
 ( #10614, #17770, #7175, #1487, #17895, #1727 ),
 ( #5272, #8947, #6945, #14208, #10847, #19918 ),
 ( #4076, #2428, #3966, #5972, #20500, #11198 ),
 ( #3730, #9408, #11437, #18471, #2186, #18253 ),
 ( #7865, #5853, #14791, #22281, #16686, #18590 ),
 ( #9645, #21941, #630, #16919, #5741, #15018 ),
 ( #12999, #15136, #13110, #22057, #11311, #22168 ),
 ( #18720, #20272, #403, #20035, #5513, #20382 ),
 ( #12760, #4202, #9184, #7753, #13224, #10968 ),
 ( #7636, #14909, #2314, #1962, #9537, #16461 ),
 ( #166, #7408, #14671, #5625, #12877, #16807 ),
 ( #20159, #3851, #11086, #18366, #519, #2077 ) ),
 .UNSPECIFIED., .F., .F., .F. ) 
 B_SPLINE_SURFACE_WITH_KNOTS ( ( 6, 3, 3, 6 ),
 ( 6, 6 ),
 ( 0.000000000000000000, 4.445608688430000122, 8.917804078430000558, 13.41780914199999941 ),
 ( 0.000000000000000000, 1.570796326505564888 ),
 .UNSPECIFIED. ) 
 GEOMETRIC_REPRESENTATION_ITEM ( )  RATIONAL_B_SPLINE_SURFACE ( (
 ( 1.000000000000000000, 0.6000000000737040207, 0.4000000000737040096, 0.3000000000552779933, 0.2500000000368520214, 0.2500000000000000000),
 ( 1.000000000000000000, 0.6000000000737040207, 0.4000000000737040096, 0.3000000000552779933, 0.2500000000368520214, 0.2500000000000000000),
 ( 1.000000000000000000, 0.6000000000737040207, 0.4000000000737040096, 0.3000000000552779933, 0.2500000000368520214, 0.2500000000000000000),
 ( 1.000000000000000000, 0.6000000000737040207, 0.4000000000737040096, 0.3000000000552779933, 0.2500000000368520214, 0.2500000000000000000),
 ( 1.000000000000000000, 0.6000000000737040207, 0.4000000000737040096, 0.3000000000552779933, 0.2500000000368520214, 0.2500000000000000000),
 ( 1.000000000000000000, 0.6000000000737040207, 0.4000000000737040096, 0.3000000000552779933, 0.2500000000368520214, 0.2500000000000000000),
 ( 1.000000000000000000, 0.6000000000737040207, 0.4000000000737040096, 0.3000000000552779933, 0.2500000000368520214, 0.2500000000000000000),
 ( 1.000000000000000000, 0.6000000000737040207, 0.4000000000737040096, 0.3000000000552779933, 0.2500000000368520214, 0.2500000000000000000),
 ( 1.000000000000000000, 0.6000000000737040207, 0.4000000000737040096, 0.3000000000552779933, 0.2500000000368520214, 0.2500000000000000000),
 ( 1.000000000000000000, 0.6000000000737040207, 0.4000000000737040096, 0.3000000000552779933, 0.2500000000368520214, 0.2500000000000000000),
 ( 1.000000000000000000, 0.6000000000737040207, 0.4000000000737040096, 0.3000000000552779933, 0.2500000000368520214, 0.2500000000000000000),
 ( 1.000000000000000000, 0.6000000000737040207, 0.4000000000737040096, 0.3000000000552779933, 0.2500000000368520214, 0.2500000000000000000) ) ) 
 REPRESENTATION_ITEM ( '' )  SURFACE ( )  );
#21944 = FILL_AREA_STYLE_COLOUR ( '', #17488 ) ;
#21945 = DIRECTION ( 'NONE',  ( 0.000000000000000000, 1.000000000000000000, -2.245315044929999938E-12 ) ) ;
#21946 = CARTESIAN_POINT ( 'NONE',  ( -13.79914019398160896, -43.91988638304457737, -150.0552959529999839 ) ) ;
#21947 = VECTOR ( 'NONE', #20513, 1000.000000000000000 ) ;
#21948 = DIRECTION ( 'NONE',  ( -0.7071067811865463515, -0.7071067811865487940, 1.591319668629388887E-12 ) ) ;
#21949 = VECTOR ( 'NONE', #9420, 1000.000000000000000 ) ;
#21950 = CARTESIAN_POINT ( 'NONE',  ( 31.00000000000000000, 39.80430157320000006, -151.0552959529999839 ) ) ;
#21951 = CONTEXT_DEPENDENT_SHAPE_REPRESENTATION ( #536, #9903 ) ;
#21952 = CARTESIAN_POINT ( 'NONE',  ( -9.334216945200001447, -17.19633444960000190, -145.5552959529999839 ) ) ;
#21953 = CARTESIAN_POINT ( 'NONE',  ( -34.50000000000000000, 48.00000000000000000, -137.5552959530000123 ) ) ;
#21954 = CARTESIAN_POINT ( 'NONE',  ( 25.50000000000000000, 22.50000000000000000, -151.0552959529999839 ) ) ;
#21955 = ORIENTED_EDGE ( 'NONE', *, *, #8152, .T. ) ;
#21956 = ORIENTED_EDGE ( 'NONE', *, *, #16789, .F. ) ;
#21957 = EDGE_CURVE ( 'NONE', #1756, #17032, #14522, .T. ) ;
#21958 = VERTEX_POINT ( 'NONE', #16758 ) ;
#21959 = DIRECTION ( 'NONE',  ( 0.000000000000000000, 0.000000000000000000, 1.000000000000000000 ) ) ;
#21960 = FACE_OUTER_BOUND ( 'NONE', #4178, .T. ) ;
#21961 = FACE_OUTER_BOUND ( 'NONE', #18474, .T. ) ;
#21962 = AXIS2_PLACEMENT_3D ( 'NONE', #2258, #13297, #4617 ) ;
#21963 = VERTEX_POINT ( 'NONE', #472 ) ;
#21964 = CARTESIAN_POINT ( 'NONE',  ( 23.17093239529999948, -15.44501179329999907, -144.5552959529999839 ) ) ;
#21965 = CARTESIAN_POINT ( 'NONE',  ( -20.40880337526489186, 35.19740419381395213, -140.3550962540792000 ) ) ;
#21966 = CARTESIAN_POINT ( 'NONE',  ( -31.00000000000000000, 47.50000000000000000, -149.0552959529999839 ) ) ;
#21967 = EDGE_LOOP ( 'NONE', ( #22692, #13078, #14950, #12541 ) ) ;
#21968 = FACE_BOUND ( 'NONE', #15080, .T. ) ;
#21969 = CARTESIAN_POINT ( 'NONE',  ( 9.563783796762269418, 38.05753333485859002, -141.7899860742832061 ) ) ;
#21970 = CARTESIAN_POINT ( 'NONE',  ( -18.18930989820000121, 36.96028804430000037, -147.6841622079999752 ) ) ;
#21971 = CARTESIAN_POINT ( 'NONE',  ( 0.5000000001340000333, 20.50000000000000000, -150.5552959529999839 ) ) ;
#21972 = EDGE_LOOP ( 'NONE', ( #10356, #19568, #21651, #17469, #7485, #9113, #6272, #8894 ) ) ;
#21973 = CIRCLE ( 'NONE', #11301, 4.000000000000003553 ) ;
#21974 = CARTESIAN_POINT ( 'NONE',  ( 6.000000000050000004, 37.00000000000000000, -146.5552959529999839 ) ) ;
#21975 = MECHANICAL_DESIGN_GEOMETRIC_PRESENTATION_REPRESENTATION (  '', ( #2228 ), #17419 ) ;
#21976 = VERTEX_POINT ( 'NONE', #7708 ) ;
#21977 = FILL_AREA_STYLE_COLOUR ( '', #19698 ) ;
#21978 = ORIENTED_EDGE ( 'NONE', *, *, #11955, .T. ) ;
#21979 = CARTESIAN_POINT ( 'NONE',  ( -25.38678224704220199, 37.07582353397776131, -140.0279244688226754 ) ) ;
#21980 = EDGE_LOOP ( 'NONE', ( #8293, #18277, #19825, #6143 ) ) ;
#21981 = EDGE_CURVE ( 'NONE', #4774, #14839, #9258, .T. ) ;
#21982 = CARTESIAN_POINT ( 'NONE',  ( -33.42928932190000069, 68.97217712079999785, -141.3604938089999905 ) ) ;
#21983 = VERTEX_POINT ( 'NONE', #20454 ) ;
#21984 = DIRECTION ( 'NONE',  ( 4.510774274160000731E-12, -1.321907670990000086E-13, 1.000000000000000000 ) ) ;
#21985 = EDGE_CURVE ( 'NONE', #11114, #8868, #3610, .T. ) ;
#21986 = ORIENTED_EDGE ( 'NONE', *, *, #6924, .T. ) ;
#21987 = VERTEX_POINT ( 'NONE', #22471 ) ;
#21988 = CARTESIAN_POINT ( 'NONE',  ( -27.38907315503255191, 40.93772549015603346, -144.3834931736647889 ) ) ;
#21989 = DIRECTION ( 'NONE',  ( 1.211690350419999855E-27, 2.765629237170000203E-27, -1.000000000000000000 ) ) ;
#21990 = CARTESIAN_POINT ( 'NONE',  ( 8.915777720172247456, 27.61753626548571106, -150.0552959529999555 ) ) ;
#21991 = CARTESIAN_POINT ( 'NONE',  ( 5.219138307789999764, -2.183626157169999971, -136.0552959530000123 ) ) ;
#21992 = CARTESIAN_POINT ( 'NONE',  ( 1.172620240290000115, -63.19354141059999108, -146.5552959529999839 ) ) ;
#21993 = AXIS2_PLACEMENT_3D ( 'NONE', #9161, #5246, #3826 ) ;
#21994 = AXIS2_PLACEMENT_3D ( 'NONE', #13282, #4255, #7807 ) ;
#21995 = CARTESIAN_POINT ( 'NONE',  ( -9.085559744729581055, 40.87064354070782457, -141.7118699073245978 ) ) ;
#21996 = EDGE_LOOP ( 'NONE', ( #3783, #20774, #17484, #8860 ) ) ;
#21997 = AXIS2_PLACEMENT_3D ( 'NONE', #1222, #19411, #4534 ) ;
#21998 = LINE ( 'NONE', #16866, #11329 ) ;
#21999 = AXIS2_PLACEMENT_3D ( 'NONE', #11094, #18600, #9193 ) ;
#22000 = CARTESIAN_POINT ( 'NONE',  ( 9.059878058829383463, 35.60814394579439579, -146.1320387297621153 ) ) ;
#22001 = VECTOR ( 'NONE', #724, 1000.000000000000000 ) ;
#22002 = ORIENTED_EDGE ( 'NONE', *, *, #19081, .F. ) ;
#22003 = CARTESIAN_POINT ( 'NONE',  ( -31.50000000000000000, 1.000000000000000000, -137.0552959530000123 ) ) ;
#22004 = ADVANCED_FACE ( 'NONE', ( #21045 ), #11500, .T. ) ;
#22006 = CARTESIAN_POINT ( 'NONE',  ( -11.80429832671256563, 38.82045246462196531, -139.9120858938445338 ) ) ;
#22005 = ADVANCED_BREP_SHAPE_REPRESENTATION ( '', ( #20016, #5025 ), #7334 ) ;
#22007 = CARTESIAN_POINT ( 'NONE',  ( 7.750000000030000002, -39.98606797749999942, -136.5552959530000123 ) ) ;
#22008 = VERTEX_POINT ( 'NONE', #17109 ) ;
#22009 = CARTESIAN_POINT ( 'NONE',  ( -9.766576661180000229, -1.500000000000000000, -145.5657682190000060 ) ) ;
#22010 = FACE_OUTER_BOUND ( 'NONE', #8043, .T. ) ;
#22011 = CIRCLE ( 'NONE', #17828, 0.7500000000000006661 ) ;
#22012 = DIRECTION ( 'NONE',  ( 1.526468026909860048E-13, 8.159623473498529972E-13, 1.000000000000000000 ) ) ;
#22013 = DIRECTION ( 'NONE',  ( 2.257144641399999941E-12, -4.009147065140000298E-51, 1.000000000000000000 ) ) ;
#22014 = CARTESIAN_POINT ( 'NONE',  ( -28.25100290369999811, 33.74243115720000219, -145.9160084049999853 ) ) ;
#22015 = CARTESIAN_POINT ( 'NONE',  ( 16.65421564080000039, -18.61497348660000029, -146.0552959529999839 ) ) ;
#22016 = VECTOR ( 'NONE', #4711, 1000.000000000000114 ) ;
#22017 = CARTESIAN_POINT ( 'NONE',  ( -19.39325354300846271, 37.07505107992977855, -139.9601895477372011 ) ) ;
#22018 = ORIENTED_EDGE ( 'NONE', *, *, #11989, .T. ) ;
#22019 = AXIS2_PLACEMENT_3D ( 'NONE', #15832, #10110, #17385 ) ;
#22020 = CARTESIAN_POINT ( 'NONE',  ( 8.750000000000000000, -39.23606797749999942, -151.0552959529999839 ) ) ;
#22021 = DIRECTION ( 'NONE',  ( 0.4289374931909490374, 0.9033341723498921061, -8.025326435147559991E-13 ) ) ;
#22022 = DIRECTION ( 'NONE',  ( 1.000000000000000000, 0.000000000000000000, -8.955190032050000935E-12 ) ) ;
#22023 = CARTESIAN_POINT ( 'NONE',  ( -21.35824191589999899, -4.750000000000000000, -146.3157682190075093 ) ) ;
#22024 = ORIENTED_EDGE ( 'NONE', *, *, #22815, .T. ) ;
#22025 = DIRECTION ( 'NONE',  ( 4.510170015240000199E-12, -1.314504061159999897E-13, 1.000000000000000000 ) ) ;
#22026 = ADVANCED_FACE ( 'NONE', ( #6517 ), #13413, .T. ) ;
#22027 = CARTESIAN_POINT ( 'NONE',  ( -15.90674982584208230, 37.04592612750105474, -148.5146100863323113 ) ) ;
#22028 = ORIENTED_EDGE ( 'NONE', *, *, #1259, .F. ) ;
#22029 = VECTOR ( 'NONE', #17163, 1000.000000000000000 ) ;
#22030 = VECTOR ( 'NONE', #8317, 1000.000000000000114 ) ;
#22031 = ORIENTED_EDGE ( 'NONE', *, *, #9777, .F. ) ;
#22032 = CIRCLE ( 'NONE', #15552, 2.500000000000002220 ) ;
#22033 = DIRECTION ( 'NONE',  ( 0.000000000000000000, 1.000000000000000000, 0.000000000000000000 ) ) ;
#22034 = ADVANCED_FACE ( 'NONE', ( #2952 ), #2726, .T. ) ;
#22035 = CARTESIAN_POINT ( 'NONE',  ( -29.13601448249999848, 36.98639052360000079, -140.5419328609999923 ) ) ;
#22036 = AXIS2_PLACEMENT_3D ( 'NONE', #14745, #22013, #1925 ) ;
#22037 = AXIS2_PLACEMENT_3D ( 'NONE', #22255, #20472, #4169 ) ;
#22038 = EDGE_CURVE ( 'NONE', #328, #23438, #11427, .T. ) ;
#22039 = CARTESIAN_POINT ( 'NONE',  ( -21.03694116389999635, 36.94210036639999828, -147.9486865819999935 ) ) ;
#22040 = CARTESIAN_POINT ( 'NONE',  ( 8.401454119002149667, 35.50000000000029843, -142.0552959529997850 ) ) ;
#22041 = VERTEX_POINT ( 'NONE', #19242 ) ;
#22042 = LINE ( 'NONE', #9395, #14331 ) ;
#22043 = LINE ( 'NONE', #9985, #15789 ) ;
#22044 = ADVANCED_FACE ( 'NONE', ( #6164 ), #7934, .T. ) ;
#22045 = CARTESIAN_POINT ( 'NONE',  ( 19.91945158500000090, 51.14507942810000429, -149.8052959529999839 ) ) ;
#22046 = CARTESIAN_POINT ( 'NONE',  ( 16.82730212879999598, -31.88969284570000084, -146.5552959529999839 ) ) ;
#22047 = EDGE_CURVE ( 'NONE', #5391, #10427, #9910, .T. ) ;
#22048 = CARTESIAN_POINT ( 'NONE',  ( -24.81028755636832273, 39.53448486588602151, -147.4801103133366382 ) ) ;
#22049 = CARTESIAN_POINT ( 'NONE',  ( -16.37184312240000139, 32.37338091950000063, -144.3414871020000021 ) ) ;
#22050 = FACE_OUTER_BOUND ( 'NONE', #27, .T. ) ;
#22051 = DIRECTION ( 'NONE',  ( 0.000000000000000000, -1.000000000000000000, 0.000000000000000000 ) ) ;
#22052 = CARTESIAN_POINT ( 'NONE',  ( -8.679997173036046121, -12.46618270809291396, -147.5552959529663610 ) ) ;
#22053 = VECTOR ( 'NONE', #13854, 1000.000000000000227 ) ;
#22054 = VECTOR ( 'NONE', #19863, 1000.000000000000000 ) ;
#22055 = VERTEX_POINT ( 'NONE', #2833 ) ;
#22056 = AXIS2_PLACEMENT_3D ( 'NONE', #9068, #11319, #14916 ) ;
#22057 = CARTESIAN_POINT ( 'NONE',  ( -6.183746982877465825, 40.52362886641058282, -144.3549557629433195 ) ) ;
#22058 = ORIENTED_EDGE ( 'NONE', *, *, #6655, .T. ) ;
#22059 = FACE_OUTER_BOUND ( 'NONE', #12700, .T. ) ;
#22060 = CARTESIAN_POINT ( 'NONE',  ( -13.50000000000000000, -43.00000000000000000, -150.0552959529999839 ) ) ;
#22061 = CARTESIAN_POINT ( 'NONE',  ( -34.35824191590000254, -1.500000000000000000, -141.0657682190000060 ) ) ;
#22062 = ORIENTED_EDGE ( 'NONE', *, *, #15296, .T. ) ;
#22063 = CARTESIAN_POINT ( 'NONE',  ( -13.71246964740000074, 35.06639867129999999, -139.8243480419999685 ) ) ;
#22064 = ADVANCED_FACE ( 'NONE', ( #16987 ), #22586, .T. ) ;
#22065 = CARTESIAN_POINT ( 'NONE',  ( 31.50000000020000002, -40.03620104850000416, -143.0552959529999839 ) ) ;
#22066 = ADVANCED_FACE ( 'NONE', ( #8285 ), #9954, .F. ) ;
#22067 = CARTESIAN_POINT ( 'NONE',  ( 12.88103053855259894, 34.98519100496140766, -150.0552959529999839 ) ) ;
#22068 = DIRECTION ( 'NONE',  ( 2.257171095940000041E-12, 1.003664318210000046E-28, 1.000000000000000000 ) ) ;
#22069 = AXIS2_PLACEMENT_3D ( 'NONE', #19255, #1637, #22838 ) ;
#22070 = DIRECTION ( 'NONE',  ( -0.9968185442904002880, 0.07970438983373201447, 8.712538262633493651E-14 ) ) ;
#22071 = VECTOR ( 'NONE', #19005, 1000.000000000000000 ) ;
#22072 = DIRECTION ( 'NONE',  ( 2.507771768019999718E-12, 1.592654864069999939E-17, -1.000000000000000000 ) ) ;
#22073 = EDGE_LOOP ( 'NONE', ( #20541, #10405, #16537, #5044 ) ) ;
#22074 = CARTESIAN_POINT ( 'NONE',  ( -27.60583033829190924, 37.01000650954619431, -148.6900182103307486 ) ) ;
#22075 = ORIENTED_EDGE ( 'NONE', *, *, #15369, .F. ) ;
#22076 = EDGE_LOOP ( 'NONE', ( #14613, #16264, #657, #12793 ) ) ;
#22077 = CARTESIAN_POINT ( 'NONE',  ( -12.28014746100000032, 36.97113097969999984, -148.4919582129999753 ) ) ;
#22078 = CARTESIAN_POINT ( 'NONE',  ( -31.75000000000000000, -36.00000000000000000, -151.0552959529999839 ) ) ;
#22079 = DIRECTION ( 'NONE',  ( -4.511946372079999833E-12, 1.314504061159999897E-13, -1.000000000000000000 ) ) ;
#22080 = ORIENTED_EDGE ( 'NONE', *, *, #9488, .F. ) ;
#22081 = CARTESIAN_POINT ( 'NONE',  ( 13.13369214859999978, 50.50000000000000000, -136.0552959530000123 ) ) ;
#22082 = CARTESIAN_POINT ( 'NONE',  ( -3.499999999969999998, 46.50000000000000000, -137.0552959530000123 ) ) ;
#22083 = CARTESIAN_POINT ( 'NONE',  ( -3.499999999969999998, 44.50000000000000000, -137.0552959530000123 ) ) ;
#22084 = AXIS2_PLACEMENT_3D ( 'NONE', #18890, #20682, #20927 ) ;
#22085 = ORIENTED_EDGE ( 'NONE', *, *, #18165, .T. ) ;
#22086 = CARTESIAN_POINT ( 'NONE',  ( -19.79184979336553241, 37.02747215728108188, -140.6521846888477114 ) ) ;
#22087 = CARTESIAN_POINT ( 'NONE',  ( 9.338338750285297252, 38.24386024261577433, -141.8866982261258727 ) ) ;
#22088 = ADVANCED_FACE ( 'NONE', ( #22825 ), #13652, .T. ) ;
#22089 = CARTESIAN_POINT ( 'NONE',  ( 7.133692148649999787, 51.50000000000000000, -137.0552959530000123 ) ) ;
#22090 = EDGE_CURVE ( 'NONE', #16889, #5668, #19436, .T. ) ;
#22091 = DIRECTION ( 'NONE',  ( 0.7071067811870332953, 0.000000000000000000, 0.7071067811860618502 ) ) ;
#22092 = ORIENTED_EDGE ( 'NONE', *, *, #10539, .T. ) ;
#22093 = DIRECTION ( 'NONE',  ( 0.000000000000000000, 0.000000000000000000, 1.000000000000000000 ) ) ;
#22094 = VERTEX_POINT ( 'NONE', #9711 ) ;
#22095 = SURFACE_STYLE_FILL_AREA ( #14602 ) ;
#22096 = VECTOR ( 'NONE', #9558, 1000.000000000000000 ) ;
#22097 = STYLED_ITEM ( 'NONE', ( #8798 ), #12179 ) ;
#22098 = VERTEX_POINT ( 'NONE', #8051 ) ;
#22099 = FACE_OUTER_BOUND ( 'NONE', #3224, .T. ) ;
#22100 = ORIENTED_EDGE ( 'NONE', *, *, #16079, .T. ) ;
#22101 = CARTESIAN_POINT ( 'NONE',  ( -23.31991597950000283, 35.31558869410000057, -140.3324749399999973 ) ) ;
#22102 = ORIENTED_EDGE ( 'NONE', *, *, #4956, .F. ) ;
#22103 = CARTESIAN_POINT ( 'NONE',  ( -13.48914305888729004, -45.62135916506274924, -150.0552959529999555 ) ) ;
#22104 = EDGE_LOOP ( 'NONE', ( #20968, #6300, #5933, #15402 ) ) ;
#22105 = ORIENTED_EDGE ( 'NONE', *, *, #2416, .T. ) ;
#22106 = CARTESIAN_POINT ( 'NONE',  ( -27.86298653490555566, 38.63966099682678390, -147.5694018320387499 ) ) ;
#22107 = APPLICATION_CONTEXT ( 'automotive_design' ) ;
#22108 = CARTESIAN_POINT ( 'NONE',  ( -14.11967125440000004, 36.98834135279999913, -140.5455248810000057 ) ) ;
#22109 = CARTESIAN_POINT ( 'NONE',  ( 14.00000000000000000, 20.50000000000000000, -150.0552959529999839 ) ) ;
#22110 = CARTESIAN_POINT ( 'NONE',  ( 29.68320006080000084, -28.50000000000000000, -148.5552959529999839 ) ) ;
#22111 = CARTESIAN_POINT ( 'NONE',  ( -6.033650297970000409, 36.94170754819999303, -147.9652040070000112 ) ) ;
#22112 = CARTESIAN_POINT ( 'NONE',  ( 24.59017985859999911, -26.91621017459999976, -148.0552959529999839 ) ) ;
#22113 = ORIENTED_EDGE ( 'NONE', *, *, #7072, .T. ) ;
#22114 = CARTESIAN_POINT ( 'NONE',  ( 7.500000000000000000, -3.500000000000000000, -145.5552959529999839 ) ) ;
#22115 = AXIS2_PLACEMENT_3D ( 'NONE', #22801, #18989, #19219 ) ;
#22116 = CIRCLE ( 'NONE', #1617, 0.7500000000000006661 ) ;
#22117 = VECTOR ( 'NONE', #747, 1000.000000000000114 ) ;
#22118 = EDGE_CURVE ( 'NONE', #16851, #16174, #15217, .T. ) ;
#22119 = CARTESIAN_POINT ( 'NONE',  ( 5.792747474889999637, -16.92794981449999980, -144.5552959529999839 ) ) ;
#22120 = EDGE_CURVE ( 'NONE', #8268, #11085, #22351, .T. ) ;
#22121 = ORIENTED_EDGE ( 'NONE', *, *, #20292, .T. ) ;
#22122 = DIRECTION ( 'NONE',  ( 0.000000000000000000, 0.000000000000000000, 1.000000000000000000 ) ) ;
#22123 = CARTESIAN_POINT ( 'NONE',  ( -10.98828237508949002, 38.00460691268780522, -139.4738624127897992 ) ) ;
#22124 = CARTESIAN_POINT ( 'NONE',  ( -17.32451618079999633, 37.89224186959999940, -139.5945780149999962 ) ) ;
#22125 = CARTESIAN_POINT ( 'NONE',  ( -29.78377644610135988, 41.56884167520560425, -144.3599435678619898 ) ) ;
#22126 = EDGE_LOOP ( 'NONE', ( #6532, #21350, #16231, #11531 ) ) ;
#22127 = PRESENTATION_STYLE_ASSIGNMENT (( #11159 ) ) ;
#22128 = FACE_OUTER_BOUND ( 'NONE', #3174, .T. ) ;
#22129 = EDGE_LOOP ( 'NONE', ( #8730, #19007, #11880, #6677 ) ) ;
#22130 = DIRECTION ( 'NONE',  ( 1.000000000000000000, 0.000000000000000000, 0.000000000000000000 ) ) ;
#22131 = CARTESIAN_POINT ( 'NONE',  ( -28.85277900879999891, 34.87340808660000135, -141.1101275619999740 ) ) ;
#22132 = CARTESIAN_POINT ( 'NONE',  ( -21.35824191589999899, -4.000000000000000000, -141.0657682190000060 ) ) ;
#22133 = CARTESIAN_POINT ( 'NONE',  ( -20.44591902742020295, 41.68207087135139943, -144.6720133961590591 ) ) ;
#22134 = COLOUR_RGB ( '', 0.72549020, 0.75294118, 0.79215686) ;
#22135 = ORIENTED_EDGE ( 'NONE', *, *, #18029, .F. ) ;
#22136 = VECTOR ( 'NONE', #11631, 1000.000000000000000 ) ;
#22137 = DIRECTION ( 'NONE',  ( 2.257749542879999954E-12, 0.000000000000000000, 1.000000000000000000 ) ) ;
#22138 = CARTESIAN_POINT ( 'NONE',  ( 32.50000000000000000, -33.03620104880000241, -137.0552959530000123 ) ) ;
#22139 = CARTESIAN_POINT ( 'NONE',  ( 15.85402906740000084, -26.57485422999999969, -146.0552959529999839 ) ) ;
#22140 = DIRECTION ( 'NONE',  ( -0.1736481776649230202, 0.000000000000000000, 0.9848077530125619594 ) ) ;
#22141 = CARTESIAN_POINT ( 'NONE',  ( -4.510008323386228923, 42.75347665030084698, -136.0552959529897805 ) ) ;
#22142 = VERTEX_POINT ( 'NONE', #15329 ) ;
#22143 = CARTESIAN_POINT ( 'NONE',  ( 2.531727043920000142, -11.80034048859999807, -148.5552959529999839 ) ) ;
#22144 = CARTESIAN_POINT ( 'NONE',  ( -32.50000000000000000, 50.00000000000000000, -150.0552959529999839 ) ) ;
#22145 = VERTEX_POINT ( 'NONE', #4270 ) ;
#22146 = COLOUR_RGB ( '', 0.66274510, 0.83137255, 0.94901961) ;
#22147 = EDGE_CURVE ( 'NONE', #20820, #6134, #2601, .T. ) ;
#22148 = ORIENTED_EDGE ( 'NONE', *, *, #12290, .F. ) ;
#22149 = VECTOR ( 'NONE', #2315, 1000.000000000000227 ) ;
#22150 = CARTESIAN_POINT ( 'NONE',  ( -22.33063748470679855, 35.38828378189443669, -140.2025093957771844 ) ) ;
#22151 = CARTESIAN_POINT ( 'NONE',  ( -29.78377644595123996, 41.56884167519815776, -144.3599435678792133 ) ) ;
#22152 = DIRECTION ( 'NONE',  ( 0.000000000000000000, 0.000000000000000000, 1.000000000000000000 ) ) ;
#22153 = CARTESIAN_POINT ( 'NONE',  ( 7.753210631989132295, 35.69821382032984047, -141.9207453427739267 ) ) ;
#22154 = ORIENTED_EDGE ( 'NONE', *, *, #17798, .T. ) ;
#22155 = CARTESIAN_POINT ( 'NONE',  ( -18.64600821076795967, 33.72696025766887828, -146.0724859999091905 ) ) ;
#22156 = PRODUCT_RELATED_PRODUCT_CATEGORY ( 'part', '', ( #21028 ) ) ;
#22157 = PLANE ( 'NONE',  #17020 ) ;
#22158 = CARTESIAN_POINT ( 'NONE',  ( 12.50006728700867242, 36.10251055748447158, -136.0552959530282351 ) ) ;
#22159 = CARTESIAN_POINT ( 'NONE',  ( -24.49703822390000241, 40.50511125069999707, -146.0729279460000214 ) ) ;
#22160 = EDGE_CURVE ( 'NONE', #16039, #20239, #14133, .T. ) ;
#22161 = CARTESIAN_POINT ( 'NONE',  ( -16.11775386688182010, 33.36946837796644161, -144.2542744048722057 ) ) ;
#22162 = DIRECTION ( 'NONE',  ( 1.000000000000000000, 0.000000000000000000, 0.000000000000000000 ) ) ;
#22163 = PLANE ( 'NONE',  #15271 ) ;
#22164 = CARTESIAN_POINT ( 'NONE',  ( 1.133692148650000009, -51.50000000000000000, -137.0552959530000123 ) ) ;
#22165 = EDGE_CURVE ( 'NONE', #21090, #1387, #21278, .T. ) ;
#22166 = B_SPLINE_CURVE_WITH_KNOTS ( 'NONE', 3,
 ( #13689, #15361, #22615, #1089, #8319, #19044, #20961, #19161, #5003, #1919 ),
 .UNSPECIFIED., .F., .F.,
 ( 4, 2, 2, 2, 4 ),
 ( 0.000000000000000000, 0.2500000000000000000, 0.5000000000000000000, 0.7500000000000000000, 1.000000000000000000 ),
 .UNSPECIFIED. ) ;
#22167 = VERTEX_POINT ( 'NONE', #15795 ) ;
#22168 = CARTESIAN_POINT ( 'NONE',  ( -6.288682382015720052, 41.28368337086639173, -144.4167712528271750 ) ) ;
#22169 = B_SPLINE_CURVE_WITH_KNOTS ( 'NONE', 3,
 ( #17862, #23447, #17736, #9026, #16311, #1451, #21682, #21, #8672, #12727 ),
 .UNSPECIFIED., .F., .F.,
 ( 4, 2, 2, 2, 4 ),
 ( 0.000000000000000000, 0.2500000000000000000, 0.5000000000000000000, 0.7500000000000000000, 1.000000000000000000 ),
 .UNSPECIFIED. ) ;
#22170 = CARTESIAN_POINT ( 'NONE',  ( -2.499999999949999996, 41.25000000000000000, -150.0552959529999839 ) ) ;
#22171 = ORIENTED_EDGE ( 'NONE', *, *, #6823, .F. ) ;
#22172 = LINE ( 'NONE', #13353, #11028 ) ;
#22173 = PLANE ( 'NONE',  #18105 ) ;
#22174 = EDGE_CURVE ( 'NONE', #17870, #3881, #7103, .T. ) ;
#22175 = CYLINDRICAL_SURFACE ( 'NONE', #12151, 4.000000000000000000 ) ;
#22176 = ORIENTED_EDGE ( 'NONE', *, *, #23054, .F. ) ;
#22177 = CARTESIAN_POINT ( 'NONE',  ( -11.99109128265850543, 36.93662743998236664, -148.3295785879953712 ) ) ;
#22178 = DIRECTION ( 'NONE',  ( 0.000000000000000000, -1.000000000000000000, 0.000000000000000000 ) ) ;
#22179 = DIRECTION ( 'NONE',  ( -1.457881434619999915E-12, -1.723066134219999902E-12, 1.000000000000000000 ) ) ;
#22180 = DIRECTION ( 'NONE',  ( 1.000000000000000000, -1.190078432789999897E-50, -2.257144641399999941E-12 ) ) ;
#22181 = CARTESIAN_POINT ( 'NONE',  ( -34.50000000000000000, 0.9999999999959999775, -155.5552959529999839 ) ) ;
#22182 = CARTESIAN_POINT ( 'NONE',  ( 4.523700915356613450, -38.03365992288669162, -150.0552959530000123 ) ) ;
#22183 = ADVANCED_FACE ( 'NONE', ( #10771 ), #1653, .F. ) ;
#22184 = EDGE_LOOP ( 'NONE', ( #3319, #6627, #5019, #21404 ) ) ;
#22185 = ADVANCED_FACE ( 'NONE', ( #1535 ), #4971, .F. ) ;
#22186 = DIRECTION ( 'NONE',  ( 0.000000000000000000, 1.000000000000000000, 0.000000000000000000 ) ) ;
#22187 = ORIENTED_EDGE ( 'NONE', *, *, #10257, .T. ) ;
#22188 =( NAMED_UNIT ( * ) PLANE_ANGLE_UNIT ( ) SI_UNIT ( $, .RADIAN. ) );
#22189 = ORIENTED_EDGE ( 'NONE', *, *, #15499, .F. ) ;
#22190 = CARTESIAN_POINT ( 'NONE',  ( -13.98445131495799387, 32.80079897227977881, -143.8357661806866474 ) ) ;
#22191 = DIRECTION ( 'NONE',  ( 0.000000000000000000, 1.000000000000000000, 0.000000000000000000 ) ) ;
#22192 = CARTESIAN_POINT ( 'NONE',  ( 29.68320006080000084, -16.50000000000000000, -149.3052959529999839 ) ) ;
#22193 = EDGE_CURVE ( 'NONE', #11758, #154, #20952, .T. ) ;
#22194 = ORIENTED_EDGE ( 'NONE', *, *, #19265, .F. ) ;
#22195 = CARTESIAN_POINT ( 'NONE',  ( 23.28059818845588680, 33.57621958799325768, -136.0552959530525641 ) ) ;
#22196 = CARTESIAN_POINT ( 'NONE',  ( 23.00000000000000000, 25.50000000000000000, -136.0552959530000123 ) ) ;
#22197 = EDGE_CURVE ( 'NONE', #21733, #15113, #9894, .T. ) ;
#22198 = ORIENTED_EDGE ( 'NONE', *, *, #22788, .T. ) ;
#22199 = CARTESIAN_POINT ( 'NONE',  ( -19.98913152175602903, 38.47389702338594475, -140.8539614082147295 ) ) ;
#22200 = ADVANCED_FACE ( 'NONE', ( #12328 ), #3421, .F. ) ;
#22201 = AXIS2_PLACEMENT_3D ( 'NONE', #19536, #8677, #17629 ) ;
#22202 = EDGE_CURVE ( 'NONE', #16936, #3124, #19605, .T. ) ;
#22203 = CARTESIAN_POINT ( 'NONE',  ( 9.499215171620216225, 38.12188228892512853, -141.8201969984096422 ) ) ;
#22204 = DIRECTION ( 'NONE',  ( 2.257749542879999954E-12, 0.000000000000000000, 1.000000000000000000 ) ) ;
#22205 = DIRECTION ( 'NONE',  ( 1.000000000000000000, -5.094701932209999624E-24, -2.257144641399999941E-12 ) ) ;
#22206 = VERTEX_POINT ( 'NONE', #6743 ) ;
#22207 = CARTESIAN_POINT ( 'NONE',  ( -3.499999999929999994, 42.50000000000000000, -138.0552959530000123 ) ) ;
#22208 = ORIENTED_EDGE ( 'NONE', *, *, #14598, .F. ) ;
#22209 = CARTESIAN_POINT ( 'NONE',  ( 5.004065293326166675, -48.00992235983122924, -150.0552959529999839 ) ) ;
#22210 = ORIENTED_EDGE ( 'NONE', *, *, #19867, .F. ) ;
#22211 = DIRECTION ( 'NONE',  ( -1.000000000000000000, 0.000000000000000000, 0.000000000000000000 ) ) ;
#22212 = ORIENTED_EDGE ( 'NONE', *, *, #10505, .T. ) ;
#22213 = AXIS2_PLACEMENT_3D ( 'NONE', #18099, #11058, #1810 ) ;
#22214 = CARTESIAN_POINT ( 'NONE',  ( -21.83347610790112014, 32.92361448676648195, -143.4947777357538143 ) ) ;
#22215 = EDGE_LOOP ( 'NONE', ( #13328, #20398, #10770, #20661 ) ) ;
#22216 = FACE_OUTER_BOUND ( 'NONE', #15322, .T. ) ;
#22217 = ORIENTED_EDGE ( 'NONE', *, *, #18782, .T. ) ;
#22218 = PRODUCT_CONTEXT ( 'NONE', #22107, 'mechanical' ) ;
#22219 = ORIENTED_EDGE ( 'NONE', *, *, #12290, .T. ) ;
#22220 = CARTESIAN_POINT ( 'NONE',  ( -27.76683509697144459, 39.35409722523485243, -147.1504185288667941 ) ) ;
#22221 = CARTESIAN_POINT ( 'NONE',  ( -32.50000000000000000, 19.50000000000000000, -150.0552959529999839 ) ) ;
#22222 = EDGE_CURVE ( 'NONE', #1341, #15103, #14114, .T. ) ;
#22223 = PLANE ( 'NONE',  #12237 ) ;
#22224 = CARTESIAN_POINT ( 'NONE',  ( -34.50000000000000000, 37.00000000000000000, -137.5552959530000123 ) ) ;
#22225 = LINE ( 'NONE', #7809, #10647 ) ;
#22226 = CARTESIAN_POINT ( 'NONE',  ( -8.810109936695118549, 39.32487244769719581, -140.7337397747917862 ) ) ;
#22227 = ORIENTED_EDGE ( 'NONE', *, *, #7732, .T. ) ;
#22228 = CARTESIAN_POINT ( 'NONE',  ( 14.00000000000000000, 20.50000000000000000, -137.0552959530000123 ) ) ;
#22229 = DIRECTION ( 'NONE',  ( -2.257157423930000049E-12, 0.000000000000000000, -1.000000000000000000 ) ) ;
#22230 = DIRECTION ( 'NONE',  ( -1.526468026909999897E-13, -8.159623473500000156E-13, -1.000000000000000000 ) ) ;
#22231 = ORIENTED_EDGE ( 'NONE', *, *, #1285, .F. ) ;
#22232 = CARTESIAN_POINT ( 'NONE',  ( 3.000000000000000000, -3.698737831368826612, -150.0552959530000408 ) ) ;
#22233 = CARTESIAN_POINT ( 'NONE',  ( -11.68432188606179700, 41.73979788245389244, -143.7054085318254693 ) ) ;
#22234 = CARTESIAN_POINT ( 'NONE',  ( 19.13369214859999801, 51.50000000000000000, -142.8052959529999839 ) ) ;
#22235 = DIRECTION ( 'NONE',  ( 2.255973186040000320E-12, 0.000000000000000000, 1.000000000000000000 ) ) ;
#22236 = VERTEX_POINT ( 'NONE', #3543 ) ;
#22237 = CARTESIAN_POINT ( 'NONE',  ( -8.514310886080000529, 36.94123471670000214, -140.1199228270000106 ) ) ;
#22238 = CARTESIAN_POINT ( 'NONE',  ( 24.55924402540000173, -29.20875385929999979, -143.5552959529999839 ) ) ;
#22239 = ORIENTED_EDGE ( 'NONE', *, *, #127, .T. ) ;
#22240 = LINE ( 'NONE', #20235, #21677 ) ;
#22241 = DIRECTION ( 'NONE',  ( 1.000000000000000000, 0.000000000000000000, 0.000000000000000000 ) ) ;
#22242 = ORIENTED_EDGE ( 'NONE', *, *, #19204, .T. ) ;
#22243 = DIRECTION ( 'NONE',  ( -7.483957154334591044E-15, 0.000000000000000000, 1.000000000000000000 ) ) ;
#22244 = CARTESIAN_POINT ( 'NONE',  ( -21.62977836625777073, 39.70709670999821128, -147.7621909749726683 ) ) ;
#22245 = ORIENTED_EDGE ( 'NONE', *, *, #21985, .F. ) ;
#22246 =( NAMED_UNIT ( * ) PLANE_ANGLE_UNIT ( ) SI_UNIT ( $, .RADIAN. ) );
#22247 = CARTESIAN_POINT ( 'NONE',  ( -27.47244207678307859, 35.09215423527204791, -148.2237751110660327 ) ) ;
#22248 = LINE ( 'NONE', #20120, #5350 ) ;
#22249 = EDGE_CURVE ( 'NONE', #328, #5806, #23293, .T. ) ;
#22250 = VERTEX_POINT ( 'NONE', #14248 ) ;
#22251 = CARTESIAN_POINT ( 'NONE',  ( 32.00000000000000000, 20.96379895120000114, -137.0552959530000123 ) ) ;
#22252 = VECTOR ( 'NONE', #6577, 1000.000000000000000 ) ;
#22253 = LINE ( 'NONE', #5944, #18723 ) ;
#22254 = CIRCLE ( 'NONE', #20369, 7.000000000000000000 ) ;
#22255 = CARTESIAN_POINT ( 'NONE',  ( 22.40884248670000289, -21.39641658300000060, -144.0552959529999839 ) ) ;
#22256 = ORIENTED_EDGE ( 'NONE', *, *, #2994, .F. ) ;
#22257 = DIRECTION ( 'NONE',  ( 0.000000000000000000, -1.000000000000000000, 8.159623473500000156E-13 ) ) ;
#22258 = PLANE ( 'NONE',  #15141 ) ;
#22259 = ORIENTED_EDGE ( 'NONE', *, *, #21023, .F. ) ;
#22260 = ORIENTED_EDGE ( 'NONE', *, *, #363, .F. ) ;
#22261 = DIRECTION ( 'NONE',  ( 2.839308199620000013E-14, 3.568879590630000244E-13, 1.000000000000000000 ) ) ;
#22262 = DIRECTION ( 'NONE',  ( 0.000000000000000000, -1.000000000000000000, 0.000000000000000000 ) ) ;
#22263 = DIRECTION ( 'NONE',  ( -2.508215857230000030E-12, 0.000000000000000000, 1.000000000000000000 ) ) ;
#22264 = CARTESIAN_POINT ( 'NONE',  ( 8.300958730110608030, 35.50974402357368831, -142.0478759868927057 ) ) ;
#22265 = VERTEX_POINT ( 'NONE', #8874 ) ;
#22266 = CARTESIAN_POINT ( 'NONE',  ( -32.00000000000000000, -50.00000000000000000, -137.0552959530000123 ) ) ;
#22267 = AXIS2_PLACEMENT_3D ( 'NONE', #22758, #13715, #6458 ) ;
#22268 = CYLINDRICAL_SURFACE ( 'NONE', #20736, 0.4999999999999936717 ) ;
#22269 = DIRECTION ( 'NONE',  ( -0.07970438983373200059, -0.9968185442904001770, 8.268372250843320857E-13 ) ) ;
#22270 = CARTESIAN_POINT ( 'NONE',  ( 14.71905350744857444, 33.57650987476316828, -136.0552959530332373 ) ) ;
#22271 = DIRECTION ( 'NONE',  ( 0.000000000000000000, 4.426606872070000353E-37, -1.000000000000000000 ) ) ;
#22272 = FACE_OUTER_BOUND ( 'NONE', #14172, .T. ) ;
#22273 = ADVANCED_FACE ( 'NONE', ( #8415 ), #5324, .F. ) ;
#22274 = CARTESIAN_POINT ( 'NONE',  ( -17.40421240568337069, 34.61091079777447987, -140.7087267687066401 ) ) ;
#22275 = DIRECTION ( 'NONE',  ( 1.000000000000000000, 0.000000000000000000, 0.000000000000000000 ) ) ;
#22276 = DIRECTION ( 'NONE',  ( 4.510774274160000731E-12, -1.321907670990000086E-13, 1.000000000000000000 ) ) ;
#22277 = EDGE_CURVE ( 'NONE', #18690, #4598, #22465, .T. ) ;
#22278 = CARTESIAN_POINT ( 'NONE',  ( -25.86630785139999844, -51.00000000000000000, -137.0552959530000123 ) ) ;
#22279 =( BOUNDED_SURFACE ( )  B_SPLINE_SURFACE ( 5, 5, ( 
 ( #17672, #10959, #10398, #9288, #19581, #1382 ),
 ( #18243, #17786, #1508, #16453, #159, #7511 ),
 ( #8731, #6961, #16561, #21135, #269, #7402 ),
 ( #4826, #4192, #20492, #18465, #510, #11426 ),
 ( #11652, #4068, #16909, #20265, #18930, #7629 ),
 ( #2178, #18710, #2643, #20613, #9525, #9873 ),
 ( #20375, #17146, #868, #9400, #11304, #7976 ),
 ( #22159, #14781, #15252, #5962, #2420, #14901 ),
 ( #17023, #22048, #4414, #22512, #16677, #13216 ),
 ( #4307, #12991, #743, #5732, #20719, #18581 ),
 ( #11537, #15010, #3957, #11190, #390, #5845 ),
 ( #13101, #6204, #2303, #7854, #15127, #22391 ) ),
 .UNSPECIFIED., .F., .F., .F. ) 
 B_SPLINE_SURFACE_WITH_KNOTS ( ( 6, 3, 3, 6 ),
 ( 6, 6 ),
 ( 0.000000000000000000, 4.509114667229999540, 8.972055907920001516, 13.39149027790000090 ),
 ( 0.000000000000000000, 1.570796326807959886 ),
 .UNSPECIFIED. ) 
 GEOMETRIC_REPRESENTATION_ITEM ( )  RATIONAL_B_SPLINE_SURFACE ( (
 ( 1.000000000000000000, 0.5999999999966999509, 0.3999999999966994957, 0.2999999999975245246, 0.2499999999983500143, 0.2500000000000000000),
 ( 1.000000000000000000, 0.5999999999966999509, 0.3999999999966994957, 0.2999999999975245246, 0.2499999999983500143, 0.2500000000000000000),
 ( 1.000000000000000000, 0.5999999999966999509, 0.3999999999966994957, 0.2999999999975245246, 0.2499999999983500143, 0.2500000000000000000),
 ( 1.000000000000000000, 0.5999999999966999509, 0.3999999999966994957, 0.2999999999975245246, 0.2499999999983500143, 0.2500000000000000000),
 ( 1.000000000000000000, 0.5999999999966999509, 0.3999999999966994957, 0.2999999999975245246, 0.2499999999983500143, 0.2500000000000000000),
 ( 1.000000000000000000, 0.5999999999966999509, 0.3999999999966994957, 0.2999999999975245246, 0.2499999999983500143, 0.2500000000000000000),
 ( 1.000000000000000000, 0.5999999999966999509, 0.3999999999966994957, 0.2999999999975245246, 0.2499999999983500143, 0.2500000000000000000),
 ( 1.000000000000000000, 0.5999999999966999509, 0.3999999999966994957, 0.2999999999975245246, 0.2499999999983500143, 0.2500000000000000000),
 ( 1.000000000000000000, 0.5999999999966999509, 0.3999999999966994957, 0.2999999999975245246, 0.2499999999983500143, 0.2500000000000000000),
 ( 1.000000000000000000, 0.5999999999966999509, 0.3999999999966994957, 0.2999999999975245246, 0.2499999999983500143, 0.2500000000000000000),
 ( 1.000000000000000000, 0.5999999999966999509, 0.3999999999966994957, 0.2999999999975245246, 0.2499999999983500143, 0.2500000000000000000),
 ( 1.000000000000000000, 0.5999999999966999509, 0.3999999999966994957, 0.2999999999975245246, 0.2499999999983500143, 0.2500000000000000000) ) ) 
 REPRESENTATION_ITEM ( '' )  SURFACE ( )  );
#22280 = ORIENTED_EDGE ( 'NONE', *, *, #13351, .F. ) ;
#22281 = CARTESIAN_POINT ( 'NONE',  ( -5.939134658313754755, 40.12020460348677631, -142.1663841678295910 ) ) ;
#22282 = FACE_BOUND ( 'NONE', #15108, .T. ) ;
#22283 = VECTOR ( 'NONE', #1378, 1000.000000000000000 ) ;
#22284 = ORIENTED_EDGE ( 'NONE', *, *, #1940, .T. ) ;
#22285 = LINE ( 'NONE', #16463, #17906 ) ;
#22286 = CARTESIAN_POINT ( 'NONE',  ( -22.83975120143743709, 33.21124457260541618, -143.6444256086801943 ) ) ;
#22287 = LINE ( 'NONE', #20509, #13259 ) ;
#22288 = ORIENTED_EDGE ( 'NONE', *, *, #11692, .T. ) ;
#22289 = CARTESIAN_POINT ( 'NONE',  ( -12.12080053524453760, 36.22692207383995822, -147.5732363758075394 ) ) ;
#22290 = CARTESIAN_POINT ( 'NONE',  ( 22.00000000000000000, -20.50000000000000000, -136.0552959530000123 ) ) ;
#22291 = DIRECTION ( 'NONE',  ( 1.000000000000000000, 0.000000000000000000, 0.000000000000000000 ) ) ;
#22292 = PLANE ( 'NONE',  #10519 ) ;
#22293 = CARTESIAN_POINT ( 'NONE',  ( 27.68320006080000084, -34.50000000000000000, -150.0552959529999839 ) ) ;
#22294 = EDGE_CURVE ( 'NONE', #12155, #7923, #8632, .T. ) ;
#22295 = DIRECTION ( 'NONE',  ( 0.7071067811866730279, -0.3390050494208429743, -0.6205445805637129775 ) ) ;
#22296 = ORIENTED_EDGE ( 'NONE', *, *, #948, .F. ) ;
#22297 = AXIS2_PLACEMENT_3D ( 'NONE', #7422, #6955, #21842 ) ;
#22298 = CARTESIAN_POINT ( 'NONE',  ( -28.89753534828613724, 32.87340430931627822, -144.5128512668707401 ) ) ;
#22299 = ORIENTED_EDGE ( 'NONE', *, *, #8625, .T. ) ;
#22300 = ORIENTED_EDGE ( 'NONE', *, *, #2250, .T. ) ;
#22301 = CARTESIAN_POINT ( 'NONE',  ( -6.093288228389445393, 36.94882630176741856, -147.6373263596331924 ) ) ;
#22302 = CARTESIAN_POINT ( 'NONE',  ( -10.15741051819999896, 33.19655140199999721, -141.5761258080000005 ) ) ;
#22303 = CARTESIAN_POINT ( 'NONE',  ( 31.50000000000000000, 32.96379895120000469, -137.0552959530000123 ) ) ;
#22304 = VERTEX_POINT ( 'NONE', #19372 ) ;
#22305 = CARTESIAN_POINT ( 'NONE',  ( -15.50000000000000000, 47.50000000000000000, -136.0552959530000123 ) ) ;
#22306 = CARTESIAN_POINT ( 'NONE',  ( -2.499999999959999997, 40.00000000000000000, -151.5552959529999839 ) ) ;
#22307 = VERTEX_POINT ( 'NONE', #3188 ) ;
#22308 = CARTESIAN_POINT ( 'NONE',  ( -20.64942635760176159, 37.69947397057557481, -140.4574076963200184 ) ) ;
#22309 = VECTOR ( 'NONE', #15904, 1000.000000000000000 ) ;
#22310 = ADVANCED_FACE ( 'NONE', ( #3077 ), #17588, .F. ) ;
#22311 = CARTESIAN_POINT ( 'NONE',  ( 8.985684983851607299, 38.42005234198289543, -141.9976801200056968 ) ) ;
#22312 = VECTOR ( 'NONE', #7043, 1000.000000000000000 ) ;
#22313 = CYLINDRICAL_SURFACE ( 'NONE', #10082, 1.500000000000001110 ) ;
#22314 = DIRECTION ( 'NONE',  ( 0.000000000000000000, 1.592654863519999645E-17, -1.000000000000000000 ) ) ;
#22315 = EDGE_LOOP ( 'NONE', ( #17244, #11508, #2350, #17420 ) ) ;
#22316 = EDGE_CURVE ( 'NONE', #16967, #73, #6864, .T. ) ;
#22317 = EDGE_CURVE ( 'NONE', #19654, #12078, #4112, .T. ) ;
#22318 = CARTESIAN_POINT ( 'NONE',  ( 15.85402906740000084, -26.57485422999999969, -146.5552959529999839 ) ) ;
#22319 = EDGE_LOOP ( 'NONE', ( #7174, #2225, #19120, #5186, #11709, #22260, #4165, #22674, #12045, #12501, #107, #23000 ) ) ;
#22320 = CARTESIAN_POINT ( 'NONE',  ( 8.750000000000000000, -47.00000000000000000, -150.0552959529999839 ) ) ;
#22321 = ADVANCED_FACE ( 'NONE', ( #7679 ), #7446, .F. ) ;
#22323 = ORIENTED_EDGE ( 'NONE', *, *, #15989, .T. ) ;
#22322 = VECTOR ( 'NONE', #732, 1000.000000000000000 ) ;
#22324 = FILL_AREA_STYLE ('',( #11710 ) ) ;
#22325 = ORIENTED_EDGE ( 'NONE', *, *, #19235, .F. ) ;
#22326 = LINE ( 'NONE', #16612, #17831 ) ;
#22327 = EDGE_CURVE ( 'NONE', #11744, #11360, #1886, .T. ) ;
#22328 = VECTOR ( 'NONE', #20107, 1000.000000000000000 ) ;
#22329 = VERTEX_POINT ( 'NONE', #21757 ) ;
#22330 = CARTESIAN_POINT ( 'NONE',  ( -12.00000000000000000, -43.00000000000000000, -150.0552959529999839 ) ) ;
#22331 = ORIENTED_EDGE ( 'NONE', *, *, #959, .F. ) ;
#22332 = EDGE_LOOP ( 'NONE', ( #18198, #7571, #2882, #5349 ) ) ;
#22333 = CARTESIAN_POINT ( 'NONE',  ( -27.45733976771897744, 41.32706283359203780, -144.4146484396392225 ) ) ;
#22334 = LINE ( 'NONE', #2588, #22793 ) ;
#22335 = CARTESIAN_POINT ( 'NONE',  ( 6.500000000000000000, 28.00000000000000000, -150.0552959529999839 ) ) ;
#22336 = CARTESIAN_POINT ( 'NONE',  ( 31.50000000000000000, -21.03620104879999886, -137.0552959530000123 ) ) ;
#22337 = CARTESIAN_POINT ( 'NONE',  ( -25.86630785129999666, -50.50000000000000000, -136.0552959530000123 ) ) ;
#22338 = CARTESIAN_POINT ( 'NONE',  ( -8.565647946481169228, 36.93510680651066025, -139.7232782068570032 ) ) ;
#22339 = EDGE_LOOP ( 'NONE', ( #23255, #22486, #20547, #13191 ) ) ;
#22340 = CARTESIAN_POINT ( 'NONE',  ( -2.499999999949999996, 40.00000000000000000, -150.0552959529999839 ) ) ;
#22341 = ADVANCED_FACE ( 'NONE', ( #201, #14947 ), #100, .T. ) ;
#22342 = VECTOR ( 'NONE', #7289, 1000.000000000000000 ) ;
#22343 = CARTESIAN_POINT ( 'NONE',  ( -46.29070078859999882, 27.75000000000000000, -147.5552959529999839 ) ) ;
#22344 = AXIS2_PLACEMENT_3D ( 'NONE', #6251, #4467, #13752 ) ;
#22345 = CARTESIAN_POINT ( 'NONE',  ( 8.500000000050000892, 37.00000000000000000, -148.0552959529999839 ) ) ;
#22346 = VERTEX_POINT ( 'NONE', #21974 ) ;
#22347 = ADVANCED_FACE ( 'NONE', ( #316 ), #438, .T. ) ;
#22348 = CARTESIAN_POINT ( 'NONE',  ( -11.47619453871935313, 38.96689531369231219, -139.6865868919825004 ) ) ;
#22349 = ADVANCED_FACE ( 'NONE', ( #1767 ), #13151, .T. ) ;
#22350 = CARTESIAN_POINT ( 'NONE',  ( -8.296392858609999976, -9.821782169089999570, -148.0552959529999839 ) ) ;
#22351 = LINE ( 'NONE', #4376, #15997 ) ;
#22352 = VERTEX_POINT ( 'NONE', #23528 ) ;
#22353 = CARTESIAN_POINT ( 'NONE',  ( -7.529689113779999943, 37.05876528330000497, -139.9906690790000141 ) ) ;
#22354 = CARTESIAN_POINT ( 'NONE',  ( -18.35824191589999899, -34.50000000000000000, -141.0657682190000060 ) ) ;
#22355 = ORIENTED_EDGE ( 'NONE', *, *, #18562, .F. ) ;
#22356 = DIRECTION ( 'NONE',  ( -1.000000000000000000, 0.000000000000000000, 2.256683728769999802E-12 ) ) ;
#22357 = DIRECTION ( 'NONE',  ( 1.211690350419999855E-27, 2.765629237170000203E-27, -1.000000000000000000 ) ) ;
#22358 = ORIENTED_EDGE ( 'NONE', *, *, #15490, .F. ) ;
#22359 = CARTESIAN_POINT ( 'NONE',  ( -32.50000000000000000, 0.000000000000000000, -150.0552959529999839 ) ) ;
#22360 = CARTESIAN_POINT ( 'NONE',  ( -21.01649482008910752, 38.86873054228240676, -148.4377912740901593 ) ) ;
#22361 = ORIENTED_EDGE ( 'NONE', *, *, #21896, .T. ) ;
#22362 =( NAMED_UNIT ( * ) SI_UNIT ( $, .STERADIAN. ) SOLID_ANGLE_UNIT ( ) );
#22363 = CARTESIAN_POINT ( 'NONE',  ( -27.36723106715751896, 36.02973761862399726, -148.4771530685680148 ) ) ;
#22364 = CIRCLE ( 'NONE', #14767, 2.500000000000000000 ) ;
#22365 = FACE_OUTER_BOUND ( 'NONE', #11501, .T. ) ;
#22366 = EDGE_LOOP ( 'NONE', ( #8105, #3100, #15857, #23432 ) ) ;
#22367 = DIRECTION ( 'NONE',  ( -0.09606172499277226828, -0.9953753789357124848, 8.289665250527615055E-13 ) ) ;
#22368 = AXIS2_PLACEMENT_3D ( 'NONE', #12483, #10807, #23329 ) ;
#22369 = DIRECTION ( 'NONE',  ( -0.1435602414469281940, -0.9896415801065048257, 3.847089866708073804E-13 ) ) ;
#22370 = CARTESIAN_POINT ( 'NONE',  ( -10.28060652870000169, 34.62853500599999990, -147.1732277810000085 ) ) ;
#22371 = EDGE_LOOP ( 'NONE', ( #20702, #14867, #8299, #3771 ) ) ;
#22372 = VECTOR ( 'NONE', #19513, 1000.000000000000000 ) ;
#22373 = DIRECTION ( 'NONE',  ( 1.000000000000000000, 0.000000000000000000, -1.522591576628786004E-13 ) ) ;
#22374 = FACE_OUTER_BOUND ( 'NONE', #18622, .T. ) ;
#22375 = ORIENTED_EDGE ( 'NONE', *, *, #17981, .T. ) ;
#22376 = EDGE_LOOP ( 'NONE', ( #9043, #9902, #7983, #7089 ) ) ;
#22377 = CARTESIAN_POINT ( 'NONE',  ( -22.52780672254771943, 37.05898997718328047, -140.0074087190062073 ) ) ;
#22378 = AXIS2_PLACEMENT_3D ( 'NONE', #3410, #5313, #17931 ) ;
#22379 = EDGE_CURVE ( 'NONE', #14539, #17914, #16391, .T. ) ;
#22380 = CARTESIAN_POINT ( 'NONE',  ( -30.02199999990120105, 40.89711431701032041, -146.3052959530037924 ) ) ;
#22381 = AXIS2_PLACEMENT_3D ( 'NONE', #6256, #18869, #11713 ) ;
#22382 = PLANE ( 'NONE',  #20422 ) ;
#22383 = DIRECTION ( 'NONE',  ( -1.000000000000000000, 0.000000000000000000, 2.257120985840000117E-12 ) ) ;
#22384 = ORIENTED_EDGE ( 'NONE', *, *, #2957, .F. ) ;
#22385 =( LENGTH_UNIT ( ) NAMED_UNIT ( * ) SI_UNIT ( .MILLI., .METRE. ) );
#22386 = CARTESIAN_POINT ( 'NONE',  ( -8.554523812450000264, 40.80811760249999764, -146.2789059460000090 ) ) ;
#22387 = CIRCLE ( 'NONE', #13646, 0.5000000000000004441 ) ;
#22388 = DIRECTION ( 'NONE',  ( 1.000000000000000000, 0.000000000000000000, -2.273736754430000208E-12 ) ) ;
#22389 = DIRECTION ( 'NONE',  ( 1.211690350419999855E-27, 2.765629237170000203E-27, -1.000000000000000000 ) ) ;
#22390 = CIRCLE ( 'NONE', #5663, 0.5000000000000004441 ) ;
#22391 = CARTESIAN_POINT ( 'NONE',  ( -24.06602356364351891, 36.94557182216171753, -148.2530914609847912 ) ) ;
#22392 = CARTESIAN_POINT ( 'NONE',  ( -15.79202522179999946, 35.03772048769999969, -148.2850092029999871 ) ) ;
#22393 = CARTESIAN_POINT ( 'NONE',  ( -17.46227293580260920, 36.22162391660916114, -140.4936808527247649 ) ) ;
#22394 = CARTESIAN_POINT ( 'NONE',  ( 23.00000000000000000, 19.50000000000000000, -150.0552959529999839 ) ) ;
#22395 = CARTESIAN_POINT ( 'NONE',  ( 13.13369214859999978, -51.50000000000000000, -136.5552959530000123 ) ) ;
#22396 = DIRECTION ( 'NONE',  ( -2.257144641399999941E-12, 8.049635416090000264E-35, -1.000000000000000000 ) ) ;
#22397 = VERTEX_POINT ( 'NONE', #3896 ) ;
#22398 = CARTESIAN_POINT ( 'NONE',  ( -9.032885736888680128, 36.94161628545133169, -147.5965110584589013 ) ) ;
#22399 = CARTESIAN_POINT ( 'NONE',  ( -29.69101630271008219, 40.01133477890059709, -145.8395111173322789 ) ) ;
#22400 = VECTOR ( 'NONE', #5695, 1000.000000000000000 ) ;
#22401 = ORIENTED_EDGE ( 'NONE', *, *, #15768, .F. ) ;
#22402 = SURFACE_SIDE_STYLE ('',( #7411 ) ) ;
#22403 = AXIS2_PLACEMENT_3D ( 'NONE', #13768, #6504, #12788 ) ;
#22404 = AXIS2_PLACEMENT_3D ( 'NONE', #6596, #15299, #22663 ) ;
#22405 = AXIS2_PLACEMENT_3D ( 'NONE', #12493, #19774, #10704 ) ;
#22406 = CARTESIAN_POINT ( 'NONE',  ( -21.95610187424196269, 33.93983213285952871, -145.7584130793499355 ) ) ;
#22407 = LINE ( 'NONE', #13357, #23162 ) ;
#22408 = VERTEX_POINT ( 'NONE', #5443 ) ;
#22409 = CARTESIAN_POINT ( 'NONE',  ( -13.13790626639999992, 32.38985286280000508, -143.7114742199999853 ) ) ;
#22410 = EDGE_CURVE ( 'NONE', #10473, #6870, #8987, .T. ) ;
#22411 = CARTESIAN_POINT ( 'NONE',  ( -17.23482902069999767, -18.00000000000000000, -146.3157682190000060 ) ) ;
#22412 = DIRECTION ( 'NONE',  ( -2.257144641399999941E-12, 0.000000000000000000, -1.000000000000000000 ) ) ;
#22413 = PLANE ( 'NONE',  #21582 ) ;
#22414 = EDGE_CURVE ( 'NONE', #23049, #13175, #10891, .T. ) ;
#22415 = CARTESIAN_POINT ( 'NONE',  ( -9.971101149720000834, 37.05360750090000721, -147.8421425029999909 ) ) ;
#22416 = CARTESIAN_POINT ( 'NONE',  ( 4.750000000000000000, -42.61803398880000060, -151.0552959529999839 ) ) ;
#22417 = ORIENTED_EDGE ( 'NONE', *, *, #13867, .F. ) ;
#22418 = AXIS2_PLACEMENT_3D ( 'NONE', #4933, #17418, #13966 ) ;
#22419 = VECTOR ( 'NONE', #7245, 1000.000000000000000 ) ;
#22420 = CARTESIAN_POINT ( 'NONE',  ( -27.26567793384627691, 36.96940380711799889, -148.4835048637780233 ) ) ;
#22421 = CIRCLE ( 'NONE', #7544, 15.00000000000000000 ) ;
#22422 = VERTEX_POINT ( 'NONE', #9332 ) ;
#22423 = CARTESIAN_POINT ( 'NONE',  ( -14.24884431179002853, 36.97292245484321427, -139.4994906131552739 ) ) ;
#22424 = DIRECTION ( 'NONE',  ( -1.701177084980000217E-20, -4.426606872460000157E-37, -1.000000000000000000 ) ) ;
#22425 = LINE ( 'NONE', #13137, #8511 ) ;
#22426 = ORIENTED_EDGE ( 'NONE', *, *, #5080, .T. ) ;
#22427 = CARTESIAN_POINT ( 'NONE',  ( 18.18320006080000084, -6.500000000000000000, -150.0552959529999839 ) ) ;
#22428 = DIRECTION ( 'NONE',  ( 2.257157423930000049E-12, 0.000000000000000000, 1.000000000000000000 ) ) ;
#22429 = ORIENTED_EDGE ( 'NONE', *, *, #3909, .F. ) ;
#22430 = CARTESIAN_POINT ( 'NONE',  ( -21.05710980616944283, 40.00468299078687551, -145.8366455853836499 ) ) ;
#22431 = CARTESIAN_POINT ( 'NONE',  ( 9.926991605570590238, 37.46297533359125964, -141.5985056068803942 ) ) ;
#22432 = VECTOR ( 'NONE', #3690, 999.9999999999998863 ) ;
#22433 = CARTESIAN_POINT ( 'NONE',  ( 3.611450600040000189E-11, -2.273736754430000208E-12, -136.0552959530000123 ) ) ;
#22434 = VECTOR ( 'NONE', #9062, 1000.000000000000000 ) ;
#22435 = CARTESIAN_POINT ( 'NONE',  ( -29.18315392570000100, -50.50000000000000000, -136.0552959530000123 ) ) ;
#22436 = CARTESIAN_POINT ( 'NONE',  ( -25.34637217103697182, 33.93854440830394026, -142.2873866648762373 ) ) ;
#22437 = ADVANCED_FACE ( 'NONE', ( #11017 ), #11234, .T. ) ;
#22438 = ORIENTED_EDGE ( 'NONE', *, *, #9236, .T. ) ;
#22439 = CARTESIAN_POINT ( 'NONE',  ( 32.50000000000000000, 32.96379895120000469, -136.0552959530000123 ) ) ;
#22440 = ORIENTED_EDGE ( 'NONE', *, *, #14055, .F. ) ;
#22441 = PLANE ( 'NONE',  #3735 ) ;
#22442 = VERTEX_POINT ( 'NONE', #19954 ) ;
#22443 = CARTESIAN_POINT ( 'NONE',  ( -27.16475626505743790, 37.90277890285160112, -148.4897851380626150 ) ) ;
#22444 = EDGE_LOOP ( 'NONE', ( #1980, #21608, #2473, #6607 ) ) ;
#22445 = CARTESIAN_POINT ( 'NONE',  ( 29.68320006080000084, 0.9999999999989999111, -148.5552959529999839 ) ) ;
#22446 = EDGE_CURVE ( 'NONE', #18676, #16549, #18294, .T. ) ;
#22447 = ORIENTED_EDGE ( 'NONE', *, *, #10655, .F. ) ;
#22448 = CARTESIAN_POINT ( 'NONE',  ( 19.68320006079999729, -24.50000000000000000, -148.5552959529999839 ) ) ;
#22449 = EDGE_LOOP ( 'NONE', ( #7518, #7154, #4320, #16401 ) ) ;
#22450 = STYLED_ITEM ( 'NONE', ( #19179 ), #11693 ) ;
#22451 = VERTEX_POINT ( 'NONE', #11126 ) ;
#22452 = CARTESIAN_POINT ( 'NONE',  ( -26.50527565025032217, 41.51083911086064404, -144.5405030845066108 ) ) ;
#22453 = CARTESIAN_POINT ( 'NONE',  ( 22.50000000000000000, 39.50000000000000000, -150.0552959529999839 ) ) ;
#22454 = DIRECTION ( 'NONE',  ( 2.256988247090000272E-12, 0.000000000000000000, 1.000000000000000000 ) ) ;
#22455 = CARTESIAN_POINT ( 'NONE',  ( -6.049191701419999845, -14.51144913589999952, -146.0552959529999839 ) ) ;
#22456 = CARTESIAN_POINT ( 'NONE',  ( -32.50000000000000000, 50.50000000000000000, -137.0552959530000123 ) ) ;
#22457 = EDGE_CURVE ( 'NONE', #20386, #3522, #9109, .T. ) ;
#22458 = CARTESIAN_POINT ( 'NONE',  ( -8.031950161270000166, 40.75709267670000457, -141.9144354160000034 ) ) ;
#22459 = ORIENTED_EDGE ( 'NONE', *, *, #16522, .T. ) ;
#22460 = EDGE_CURVE ( 'NONE', #4685, #4452, #2227, .T. ) ;
#22461 = LINE ( 'NONE', #13172, #17429 ) ;
#22462 = EDGE_CURVE ( 'NONE', #22008, #15711, #5782, .T. ) ;
#22463 = CARTESIAN_POINT ( 'NONE',  ( -14.50908993389082724, 36.94185792195812468, -140.4668331869691826 ) ) ;
#22464 = CARTESIAN_POINT ( 'NONE',  ( 3.579771545658129828, -2.298869075814014451, -136.0552959530081125 ) ) ;
#22465 = CIRCLE ( 'NONE', #10295, 5.000000000000000000 ) ;
#22466 = EDGE_LOOP ( 'NONE', ( #19043, #7867, #19931, #17236 ) ) ;
#22467 = VECTOR ( 'NONE', #2449, 1000.000000000000000 ) ;
#22468 = CIRCLE ( 'NONE', #443, 3.500000000000000000 ) ;
#22469 = CARTESIAN_POINT ( 'NONE',  ( -11.86129685666417544, 38.63195145382516671, -140.3074378722488689 ) ) ;
#22470 = CARTESIAN_POINT ( 'NONE',  ( -17.89449017619289961, 39.21037955095951588, -147.0820833684587967 ) ) ;
#22471 = CARTESIAN_POINT ( 'NONE',  ( 25.50000000000000000, 19.50000000000000000, -137.0552959530000123 ) ) ;
#22472 = EDGE_LOOP ( 'NONE', ( #13680, #21827, #16604, #7319, #5564 ) ) ;
#22473 = CARTESIAN_POINT ( 'NONE',  ( 11.53320006080000049, -24.50000000000000000, -150.0552959529999839 ) ) ;
#22474 = ORIENTED_EDGE ( 'NONE', *, *, #9384, .T. ) ;
#22475 = LINE ( 'NONE', #20687, #14817 ) ;
#22476 = DIRECTION ( 'NONE',  ( -1.000000000000000000, 0.000000000000000000, 0.000000000000000000 ) ) ;
#22477 = ORIENTED_EDGE ( 'NONE', *, *, #4032, .F. ) ;
#22478 = CARTESIAN_POINT ( 'NONE',  ( -8.734077015120000453, -11.22642389220000148, -146.5552959529999839 ) ) ;
#22479 = EDGE_CURVE ( 'NONE', #9295, #16366, #16726, .T. ) ;
#22480 = CARTESIAN_POINT ( 'NONE',  ( -21.29590688489999906, 41.28591597809999314, -144.5271551099999954 ) ) ;
#22481 = ORIENTED_EDGE ( 'NONE', *, *, #22165, .T. ) ;
#22482 = FILL_AREA_STYLE ('',( #2272 ) ) ;
#22483 = EDGE_CURVE ( 'NONE', #10783, #17304, #796, .T. ) ;
#22484 = CARTESIAN_POINT ( 'NONE',  ( -28.71558688633279743, 36.31472216850572465, -140.6134838335071890 ) ) ;
#22485 = LINE ( 'NONE', #23279, #5718 ) ;
#22486 = ORIENTED_EDGE ( 'NONE', *, *, #17610, .F. ) ;
#22487 = CARTESIAN_POINT ( 'NONE',  ( -13.92432874550000044, 37.01165864720000087, -139.5650670249999905 ) ) ;
#22488 = LINE ( 'NONE', #18559, #20609 ) ;
#22489 = ORIENTED_EDGE ( 'NONE', *, *, #608, .F. ) ;
#22490 = VECTOR ( 'NONE', #2641, 1000.000000000000000 ) ;
#22491 = AXIS2_PLACEMENT_3D ( 'NONE', #20153, #20268, #16804 ) ;
#22492 = AXIS2_PLACEMENT_3D ( 'NONE', #10728, #1723, #18246 ) ;
#22493 = EDGE_LOOP ( 'NONE', ( #2742, #12446 ) ) ;
#22494 = ADVANCED_FACE ( 'NONE', ( #7902 ), #13954, .T. ) ;
#22495 = CARTESIAN_POINT ( 'NONE',  ( -9.394779979509999990, -17.86685386420000299, -142.5552959529999839 ) ) ;
#22496 = EDGE_CURVE ( 'NONE', #4521, #18822, #21226, .T. ) ;
#22497 = LINE ( 'NONE', #14885, #19695 ) ;
#22498 = ORIENTED_EDGE ( 'NONE', *, *, #368, .F. ) ;
#22499 = ADVANCED_FACE ( 'NONE', ( #15304 ), #23121, .F. ) ;
#22500 = EDGE_LOOP ( 'NONE', ( #9983, #23088, #8162, #2958 ) ) ;
#22501 = PLANE ( 'NONE',  #15445 ) ;
#22502 = DIRECTION ( 'NONE',  ( -1.525446435830000185E-13, -8.171241461240000022E-13, -1.000000000000000000 ) ) ;
#22503 = LINE ( 'NONE', #613, #15107 ) ;
#22504 = DIRECTION ( 'NONE',  ( -0.1000233216789610108, -0.9949850929136109245, 3.576398436658600095E-13 ) ) ;
#22505 = VERTEX_POINT ( 'NONE', #22318 ) ;
#22506 = CIRCLE ( 'NONE', #11830, 3.000000000000000888 ) ;
#22507 = VECTOR ( 'NONE', #2125, 1000.000000000000114 ) ;
#22508 = DIRECTION ( 'NONE',  ( -0.9913873220698726785, 0.1309625047069831461, -1.853446743629759619E-14 ) ) ;
#22509 = VECTOR ( 'NONE', #571, 1000.000000000000000 ) ;
#22510 = DIRECTION ( 'NONE',  ( 0.000000000000000000, 0.000000000000000000, -1.000000000000000000 ) ) ;
#22511 = DIRECTION ( 'NONE',  ( -0.9892101392001054760, 0.1465035852930155480, 4.471739159800472250E-12 ) ) ;
#22512 = CARTESIAN_POINT ( 'NONE',  ( -24.31845739552116825, 39.82285914874432819, -147.9810288385895944 ) ) ;
#22513 = CARTESIAN_POINT ( 'NONE',  ( -15.76532943048110091, 34.76918918228179933, -146.9254579970016152 ) ) ;
#22514 = CARTESIAN_POINT ( 'NONE',  ( -16.90879464662080878, 32.79049683898814749, -144.3773178752514355 ) ) ;
#22515 = CYLINDRICAL_SURFACE ( 'NONE', #14533, 0.7500000000000006661 ) ;
#22516 = DIRECTION ( 'NONE',  ( 1.000000000000000000, 0.000000000000000000, 0.000000000000000000 ) ) ;
#22517 = DIRECTION ( 'NONE',  ( 1.000000000000000000, 0.000000000000000000, -2.257453483404485639E-12 ) ) ;
#22518 = ORIENTED_EDGE ( 'NONE', *, *, #5801, .F. ) ;
#22519 = CARTESIAN_POINT ( 'NONE',  ( -10.01905152896493512, 33.53823069094890741, -144.2070255763365765 ) ) ;
#22520 = CARTESIAN_POINT ( 'NONE',  ( 29.68320006080000084, -32.50000000000000000, -149.3052959529999839 ) ) ;
#22521 = ADVANCED_FACE ( 'NONE', ( #7789 ), #22560, .T. ) ;
#22522 = DIRECTION ( 'NONE',  ( 1.000000000000000000, 0.000000000000000000, 0.000000000000000000 ) ) ;
#22523 = PRESENTATION_LAYER_ASSIGNMENT (  '', '', ( #11103 ) ) ;
#22524 = VERTEX_POINT ( 'NONE', #11354 ) ;
#22525 = AXIS2_PLACEMENT_3D ( 'NONE', #1043, #6617, #6150 ) ;
#22526 = CARTESIAN_POINT ( 'NONE',  ( -21.41277927229678824, 34.79026080032429746, -146.9436551339746302 ) ) ;
#22527 = CARTESIAN_POINT ( 'NONE',  ( -34.50000000000000000, -74.00000000000000000, -155.5552959529999839 ) ) ;
#22528 = EDGE_LOOP ( 'NONE', ( #22075, #17323, #3212, #14504, #21745, #15017, #11525, #5150, #7425, #4096, #18862, #9508, #2671, #9805, #18918, #2122, #9097 ) ) ;
#22529 = LINE ( 'NONE', #11446, #4159 ) ;
#22530 = DIRECTION ( 'NONE',  ( 2.257171095940000041E-12, 1.003664318210000046E-28, 1.000000000000000000 ) ) ;
#22531 = DIRECTION ( 'NONE',  ( 2.602084747549999882E-17, -1.000000000000000000, -5.873289694040000105E-29 ) ) ;
#22532 = DIRECTION ( 'NONE',  ( -3.994014902950000436E-29, 1.000000000000000000, -4.148443855749999753E-27 ) ) ;
#22533 = ADVANCED_FACE ( 'NONE', ( #4238 ), #13266, .T. ) ;
#22534 = DIRECTION ( 'NONE',  ( 0.000000000000000000, -1.000000000000000000, 0.000000000000000000 ) ) ;
#22535 = CARTESIAN_POINT ( 'NONE',  ( -10.14042191033887086, 37.07381867794360630, -148.2039739395296749 ) ) ;
#22536 = CARTESIAN_POINT ( 'NONE',  ( -7.728596210859999260, 38.74386132360000090, -140.2295773360000055 ) ) ;
#22537 = VERTEX_POINT ( 'NONE', #6694 ) ;
#22538 = CARTESIAN_POINT ( 'NONE',  ( -8.665242998822469289, -11.36832253183628616, -144.5552959529994439 ) ) ;
#22539 = ORIENTED_EDGE ( 'NONE', *, *, #18484, .F. ) ;
#22540 = CARTESIAN_POINT ( 'NONE',  ( -13.46508678921569313, 33.00136909151063236, -146.5816114374932226 ) ) ;
#22541 = FACE_OUTER_BOUND ( 'NONE', #22315, .T. ) ;
#22542 = EDGE_CURVE ( 'NONE', #14976, #3870, #6812, .T. ) ;
#22543 = DIRECTION ( 'NONE',  ( 1.000000000000000000, 0.000000000000000000, -2.258578509400000305E-12 ) ) ;
#22544 = ADVANCED_FACE ( 'NONE', ( #12044 ), #6249, .T. ) ;
#22545 = EDGE_LOOP ( 'NONE', ( #9888, #7680, #295, #8481 ) ) ;
#22546 = EDGE_CURVE ( 'NONE', #12137, #3906, #9799, .T. ) ;
#22547 = LINE ( 'NONE', #6825, #7220 ) ;
#22548 = DIRECTION ( 'NONE',  ( 2.256861364460000137E-12, 0.000000000000000000, 1.000000000000000000 ) ) ;
#22549 = EDGE_CURVE ( 'NONE', #19018, #13428, #13499, .T. ) ;
#22550 = VERTEX_POINT ( 'NONE', #19313 ) ;
#22551 = CARTESIAN_POINT ( 'NONE',  ( -21.19302672506264429, 40.61567049807046459, -143.6742535173994781 ) ) ;
#22552 = CARTESIAN_POINT ( 'NONE',  ( -17.27864984443349883, 40.23496799371888244, -142.1532139957071763 ) ) ;
#22553 = VERTEX_POINT ( 'NONE', #18867 ) ;
#22554 = CARTESIAN_POINT ( 'NONE',  ( 6.500000000030000002, 28.00000000000000000, -136.5552959530000123 ) ) ;
#22555 = CARTESIAN_POINT ( 'NONE',  ( 4.500000000009999113, -3.500000000000000000, -136.0552959530000123 ) ) ;
#22556 = APPLICATION_CONTEXT ( 'automotive_design' ) ;
#22557 = CARTESIAN_POINT ( 'NONE',  ( -26.29566636579999894, 36.18167175180000328, -140.3932108110000172 ) ) ;
#22558 = EDGE_LOOP ( 'NONE', ( #13022, #4294, #4124, #22092, #7048 ) ) ;
#22559 =( BOUNDED_CURVE ( )  B_SPLINE_CURVE ( 5, ( #17720, #17609, #19514, #14031, #15584, #4752, #15815, #10088, #8541, #22966, #1431, #8653 ),
 .UNSPECIFIED., .F., .F. ) 
 B_SPLINE_CURVE_WITH_KNOTS ( ( 6, 3, 3, 6 ),
 ( 0.000000000000000000, 4.454241660750000165, 8.943513424000000711, 13.47090878500000066 ),
 .UNSPECIFIED. ) 
 CURVE ( )  GEOMETRIC_REPRESENTATION_ITEM ( )  RATIONAL_B_SPLINE_CURVE ( ( 0.2500000000000000000, 0.2500000000000000000, 0.2500000000000000000, 0.2500000000000000000, 0.2500000000000000000, 0.2500000000000000000, 0.2500000000000000000, 0.2500000000000000000, 0.2500000000000000000, 0.2500000000000000000, 0.2500000000000000000, 0.2500000000000000000 ) ) 
 REPRESENTATION_ITEM ( '' )  );
#22560 = PLANE ( 'NONE',  #15253 ) ;
#22561 = EDGE_LOOP ( 'NONE', ( #22331, #2185, #4625, #3818, #1902, #17587, #18996, #5507, #1987, #21286, #2078 ) ) ;
#22562 = PLANE ( 'NONE',  #19306 ) ;
#22563 = ORIENTED_EDGE ( 'NONE', *, *, #5889, .F. ) ;
#22564 = ORIENTED_EDGE ( 'NONE', *, *, #2129, .T. ) ;
#22565 = CARTESIAN_POINT ( 'NONE',  ( -7.520331543250000195, 50.50000000000000000, -136.0552959530000123 ) ) ;
#22566 = ORIENTED_EDGE ( 'NONE', *, *, #14869, .F. ) ;
#22567 = CARTESIAN_POINT ( 'NONE',  ( -4.499999999949999996, 32.75000000000000000, -150.0552959529999839 ) ) ;
#22568 = VERTEX_POINT ( 'NONE', #8476 ) ;
#22569 = ORIENTED_EDGE ( 'NONE', *, *, #18621, .T. ) ;
#22570 = EDGE_CURVE ( 'NONE', #19702, #5769, #3027, .T. ) ;
#22571 = VECTOR ( 'NONE', #18386, 1000.000000000000000 ) ;
#22572 = DIRECTION ( 'NONE',  ( 1.000000000000000000, -5.094701941669999797E-24, -2.257144641399999941E-12 ) ) ;
#22573 = LINE ( 'NONE', #11369, #7579 ) ;
#22574 = CARTESIAN_POINT ( 'NONE',  ( 8.900000000049999471, 34.53220746410000430, -149.5552959529999839 ) ) ;
#22575 = EDGE_CURVE ( 'NONE', #2789, #3632, #10372, .T. ) ;
#22576 = SURFACE_STYLE_FILL_AREA ( #10301 ) ;
#22577 = CARTESIAN_POINT ( 'NONE',  ( -35.47299999999999898, 16.95803989150000035, -144.5552959529999839 ) ) ;
#22578 = CARTESIAN_POINT ( 'NONE',  ( -9.112817567394211338, 37.91675322417339089, -148.5775373212531463 ) ) ;
#22579 = EDGE_LOOP ( 'NONE', ( #878, #4025, #14926, #7458 ) ) ;
#22580 = CARTESIAN_POINT ( 'NONE',  ( -27.26567793380000282, 36.96940380710000085, -148.4835048639999968 ) ) ;
#22581 = PLANE ( 'NONE',  #9826 ) ;
#22582 = LINE ( 'NONE', #8161, #5309 ) ;
#22583 = ORIENTED_EDGE ( 'NONE', *, *, #21808, .T. ) ;
#22584 = VECTOR ( 'NONE', #22629, 1000.000000000000000 ) ;
#22585 = CARTESIAN_POINT ( 'NONE',  ( -17.53569647182064273, 40.68917497046800236, -144.4123951040203906 ) ) ;
#22586 = PLANE ( 'NONE',  #20190 ) ;
#22587 = ORIENTED_EDGE ( 'NONE', *, *, #14577, .F. ) ;
#22588 = CARTESIAN_POINT ( 'NONE',  ( 8.750000000030000891, -35.98606797749999942, -136.5552959530000123 ) ) ;
#22589 = EDGE_CURVE ( 'NONE', #15515, #1861, #9574, .T. ) ;
#22590 = VERTEX_POINT ( 'NONE', #16848 ) ;
#22591 = DIRECTION ( 'NONE',  ( -1.211690350419999855E-27, -2.765629237170000203E-27, 1.000000000000000000 ) ) ;
#22592 = CARTESIAN_POINT ( 'NONE',  ( 22.71475634692216516, -23.42191803000494588, -150.0552959529999839 ) ) ;
#22593 = VERTEX_POINT ( 'NONE', #4352 ) ;
#22594 = CARTESIAN_POINT ( 'NONE',  ( -14.40511015809376083, 39.11695720674963894, -141.1121292871317792 ) ) ;
#22595 = CARTESIAN_POINT ( 'NONE',  ( -25.11959125024334227, 32.26208325171451463, -143.5588604866181015 ) ) ;
#22596 = EDGE_LOOP ( 'NONE', ( #16826, #22604, #10324, #20231 ) ) ;
#22597 = FACE_OUTER_BOUND ( 'NONE', #19131, .T. ) ;
#22598 = VERTEX_POINT ( 'NONE', #22439 ) ;
#22599 = LINE ( 'NONE', #13429, #12115 ) ;
#22600 = CARTESIAN_POINT ( 'NONE',  ( -15.50000000000000000, -2.273736754430000208E-12, -136.0552959530000123 ) ) ;
#22601 = ORIENTED_EDGE ( 'NONE', *, *, #8799, .F. ) ;
#22602 = EDGE_CURVE ( 'NONE', #8980, #17699, #17531, .T. ) ;
#22603 = DIRECTION ( 'NONE',  ( -1.527666881879999979E-13, -8.153477892850000134E-13, -1.000000000000000000 ) ) ;
#22604 = ORIENTED_EDGE ( 'NONE', *, *, #20797, .F. ) ;
#22605 = CARTESIAN_POINT ( 'NONE',  ( 11.68320006080000262, -20.36749606047844807, -148.5552959529999839 ) ) ;
#22606 = CYLINDRICAL_SURFACE ( 'NONE', #18188, 2.000000000000001776 ) ;
#22607 = VERTEX_POINT ( 'NONE', #13388 ) ;
#22608 = EDGE_CURVE ( 'NONE', #21873, #6936, #2352, .T. ) ;
#22609 = ORIENTED_EDGE ( 'NONE', *, *, #20743, .F. ) ;
#22610 = DIRECTION ( 'NONE',  ( -1.000000000000000000, -3.994014902950000436E-29, 0.000000000000000000 ) ) ;
#22611 = DIRECTION ( 'NONE',  ( 0.000000000000000000, 0.000000000000000000, 1.000000000000000000 ) ) ;
#22612 = CARTESIAN_POINT ( 'NONE',  ( 8.500000000060001781, 37.00000000000000000, -144.0552959529999839 ) ) ;
#22613 = CARTESIAN_POINT ( 'NONE',  ( 31.50000000000000000, -21.03620104879999886, -136.0552959530000123 ) ) ;
#22614 = EDGE_LOOP ( 'NONE', ( #6175, #18516, #22678, #996 ) ) ;
#22615 = CARTESIAN_POINT ( 'NONE',  ( -16.46175622020525608, -42.60932014324554018, -136.0552959529628367 ) ) ;
#22616 = DIRECTION ( 'NONE',  ( 0.04856869991388110264, 0.9988198443106121038, -3.578457907868606044E-13 ) ) ;
#22617 = EDGE_CURVE ( 'NONE', #4666, #20239, #12378, .T. ) ;
#22618 = LINE ( 'NONE', #6202, #13981 ) ;
#22619 = DIRECTION ( 'NONE',  ( 1.000000000000000000, 2.602084704497994558E-17, -1.701177080612860179E-20 ) ) ;
#22620 = DIRECTION ( 'NONE',  ( 2.257157423930000049E-12, 0.000000000000000000, 1.000000000000000000 ) ) ;
#22621 = ADVANCED_FACE ( 'NONE', ( #14196 ), #3719, .T. ) ;
#22622 = VECTOR ( 'NONE', #4411, 1000.000000000000000 ) ;
#22623 = CARTESIAN_POINT ( 'NONE',  ( -16.06125683602935084, 34.67123563680174669, -140.5203502863974165 ) ) ;
#22624 = ADVANCED_FACE ( 'NONE', ( #16217 ), #14663, .T. ) ;
#22625 = CARTESIAN_POINT ( 'NONE',  ( -17.01097330534292240, 32.84288031327549362, -143.4865848381450348 ) ) ;
#22626 = EDGE_CURVE ( 'NONE', #1030, #4038, #14431, .T. ) ;
#22627 = CARTESIAN_POINT ( 'NONE',  ( -4.428060343052305114, 37.07089632425688563, -139.9976721173915450 ) ) ;
#22628 = DIRECTION ( 'NONE',  ( 8.955190032050000935E-12, -9.104778821549999739E-13, 1.000000000000000000 ) ) ;
#22629 = DIRECTION ( 'NONE',  ( -0.1435602414469281940, -0.9896415801065048257, 3.849849731938073961E-13 ) ) ;
#22630 = ORIENTED_EDGE ( 'NONE', *, *, #7780, .F. ) ;
#22631 = CARTESIAN_POINT ( 'NONE',  ( 23.93619342817335394, -31.59589658247995203, -143.5552959530006660 ) ) ;
#22632 = LINE ( 'NONE', #18939, #14166 ) ;
#22633 = DIRECTION ( 'NONE',  ( 1.000000000000000000, 0.000000000000000000, 0.000000000000000000 ) ) ;
#22634 = ORIENTED_EDGE ( 'NONE', *, *, #792, .F. ) ;
#22635 = LINE ( 'NONE', #21095, #45 ) ;
#22637 = AXIS2_PLACEMENT_3D ( 'NONE', #5757, #20284, #414 ) ;
#22636 = DIRECTION ( 'NONE',  ( 0.000000000000000000, -4.148443855749999753E-27, -1.000000000000000000 ) ) ;
#22638 = VECTOR ( 'NONE', #19334, 1000.000000000000000 ) ;
#22639 = CARTESIAN_POINT ( 'NONE',  ( 9.683200060759999062, -20.50000000000000000, -150.0552959529999839 ) ) ;
#22640 = ORIENTED_EDGE ( 'NONE', *, *, #17951, .F. ) ;
#22641 = CARTESIAN_POINT ( 'NONE',  ( -22.52780672254944250, 37.05898997718308152, -140.0074087189881880 ) ) ;
#22642 = CARTESIAN_POINT ( 'NONE',  ( -16.81794493339999619, 37.02435727940000731, -140.5111119820000170 ) ) ;
#22643 = CARTESIAN_POINT ( 'NONE',  ( 0.8488229453495553800, 15.54483228932120120, -150.0552959529999839 ) ) ;
#22644 = DIRECTION ( 'NONE',  ( 0.000000000000000000, 0.000000000000000000, 1.000000000000000000 ) ) ;
#22645 = CARTESIAN_POINT ( 'NONE',  ( -5.733381482170000432, 39.34803470290000149, -147.3316303149999840 ) ) ;
#22646 = DIRECTION ( 'NONE',  ( -1.211690350419999855E-27, -2.765629237170000203E-27, 1.000000000000000000 ) ) ;
#22647 = CARTESIAN_POINT ( 'NONE',  ( -8.238646733050000392, 41.24792906369999912, -143.6196368420000056 ) ) ;
#22648 = EDGE_LOOP ( 'NONE', ( #8526, #15330, #19093, #6736 ) ) ;
#22649 = EDGE_CURVE ( 'NONE', #20697, #12372, #16336, .T. ) ;
#22650 = EDGE_LOOP ( 'NONE', ( #9831, #5949, #15698, #15398 ) ) ;
#22651 = PRODUCT_DEFINITION_SHAPE ( 'NONE', 'NONE',  #23552 ) ;
#22652 = VECTOR ( 'NONE', #19525, 1000.000000000000000 ) ;
#22653 = CARTESIAN_POINT ( 'NONE',  ( -13.44992991213783995, 32.27235479864616963, -143.7382959716714481 ) ) ;
#22654 = CARTESIAN_POINT ( 'NONE',  ( 6.500000000000000000, 20.50000000000000000, -151.0552959529999839 ) ) ;
#22655 = AXIS2_PLACEMENT_3D ( 'NONE', #20631, #18729, #22178 ) ;
#22656 = LINE ( 'NONE', #15396, #14606 ) ;
#22657 = ORIENTED_EDGE ( 'NONE', *, *, #5080, .F. ) ;
#22658 = DIRECTION ( 'NONE',  ( 4.430318231639999944E-12, -6.100259101500000139E-13, 1.000000000000000000 ) ) ;
#22659 = CARTESIAN_POINT ( 'NONE',  ( -14.68945449529999969, 41.62249060810000145, -143.5408288559999903 ) ) ;
#22660 = VERTEX_POINT ( 'NONE', #10836 ) ;
#22661 = CARTESIAN_POINT ( 'NONE',  ( 9.183200060760000838, 0.4999999999990000776, -150.0552959529999839 ) ) ;
#22662 = CARTESIAN_POINT ( 'NONE',  ( -19.04747499291816482, 37.87694391812206618, -147.8065290023580189 ) ) ;
#22663 = DIRECTION ( 'NONE',  ( -1.000000000000000000, 0.000000000000000000, 1.701177084980000217E-20 ) ) ;
#22664 = DIRECTION ( 'NONE',  ( 1.000000000000000000, 0.000000000000000000, 0.000000000000000000 ) ) ;
#22665 = VECTOR ( 'NONE', #23023, 1000.000000000000227 ) ;
#22666 = CARTESIAN_POINT ( 'NONE',  ( -25.30721887416896010, 33.85380199680784585, -145.9318938156505965 ) ) ;
#22667 = CARTESIAN_POINT ( 'NONE',  ( 0.000000000000000000, 33.50000000000000000, -150.0552959529999839 ) ) ;
#22668 = EDGE_CURVE ( 'NONE', #19806, #17304, #21703, .T. ) ;
#22669 = ORIENTED_EDGE ( 'NONE', *, *, #6232, .F. ) ;
#22670 = DIRECTION ( 'NONE',  ( 0.000000000000000000, -0.4794255386042033384, -0.8775825618903726477 ) ) ;
#22671 = ADVANCED_FACE ( 'NONE', ( #1604 ), #23357, .F. ) ;
#22672 = EDGE_LOOP ( 'NONE', ( #20157, #4835, #20565, #19789 ) ) ;
#22673 = CARTESIAN_POINT ( 'NONE',  ( -27.39460866327015864, 37.71341861930930150, -147.4556575159825229 ) ) ;
#22674 = ORIENTED_EDGE ( 'NONE', *, *, #2220, .F. ) ;
#22675 = DIRECTION ( 'NONE',  ( 0.3704939739869947957, -0.9288348697369861462, -4.163336342344337834E-12 ) ) ;
#22676 = EDGE_LOOP ( 'NONE', ( #17408, #14464, #10635, #12934 ) ) ;
#22677 = PLANE ( 'NONE',  #11764 ) ;
#22678 = ORIENTED_EDGE ( 'NONE', *, *, #5211, .T. ) ;
#22679 = VECTOR ( 'NONE', #22179, 1000.000000000000000 ) ;
#22680 = ORIENTED_EDGE ( 'NONE', *, *, #21448, .F. ) ;
#22681 = DIRECTION ( 'NONE',  ( 0.000000000000000000, -1.000000000000000000, 0.000000000000000000 ) ) ;
#22682 = LINE ( 'NONE', #11962, #3431 ) ;
#22683 = CARTESIAN_POINT ( 'NONE',  ( 23.50000000000000000, -20.50000000000000000, -135.0552959530000123 ) ) ;
#22684 = DIRECTION ( 'NONE',  ( -1.000000000000000000, 0.000000000000000000, 0.000000000000000000 ) ) ;
#22685 = CARTESIAN_POINT ( 'NONE',  ( -7.469704578253070437, 36.11012087976002505, -139.6489141305654584 ) ) ;
#22686 = CARTESIAN_POINT ( 'NONE',  ( -8.764836022000000781, 39.53398178709999655, -147.5842891229999907 ) ) ;
#22687 = ORIENTED_EDGE ( 'NONE', *, *, #19616, .T. ) ;
#22688 = DIRECTION ( 'NONE',  ( 0.000000000000000000, -1.000000000000000000, 0.000000000000000000 ) ) ;
#22689 =( BOUNDED_CURVE ( )  B_SPLINE_CURVE ( 5, ( #22108, #14960, #9587, #5795, #13055, #20327, #2476, #15074, #6027, #17326, #17799, #3066 ),
 .UNSPECIFIED., .F., .F. ) 
 B_SPLINE_CURVE_WITH_KNOTS ( ( 6, 3, 3, 6 ),
 ( 0.000000000000000000, 4.151671928079999851, 8.316542232069998875, 12.50501063799999990 ),
 .UNSPECIFIED. ) 
 CURVE ( )  GEOMETRIC_REPRESENTATION_ITEM ( )  RATIONAL_B_SPLINE_CURVE ( ( 0.2500000000000000000, 0.2500000000000000000, 0.2500000000000000000, 0.2500000000000000000, 0.2500000000000000000, 0.2500000000000000000, 0.2500000000000000000, 0.2500000000000000000, 0.2500000000000000000, 0.2500000000000000000, 0.2500000000000000000, 0.2500000000000000000 ) ) 
 REPRESENTATION_ITEM ( '' )  );
#22690 = CARTESIAN_POINT ( 'NONE',  ( 7.133692148649999787, -51.50000000000000000, -137.0552959530000123 ) ) ;
#22691 = CARTESIAN_POINT ( 'NONE',  ( 24.01462304342504339, 39.11919234682564195, -150.0552959530000123 ) ) ;
#22692 = ORIENTED_EDGE ( 'NONE', *, *, #1313, .T. ) ;
#22693 = VECTOR ( 'NONE', #19819, 1000.000000000000000 ) ;
#22694 = EDGE_CURVE ( 'NONE', #14260, #5200, #5504, .T. ) ;
#22695 = CARTESIAN_POINT ( 'NONE',  ( -18.50695094929572804, 37.98868281441455252, -148.6476439268063245 ) ) ;
#22696 = DIRECTION ( 'NONE',  ( -1.000000000000000000, 0.000000000000000000, 2.257453483404484831E-12 ) ) ;
#22697 = CIRCLE ( 'NONE', #11288, 8.000000000000000000 ) ;
#22698 = ORIENTED_EDGE ( 'NONE', *, *, #377, .F. ) ;
#22699 = CARTESIAN_POINT ( 'NONE',  ( 10.68320006080000084, -20.50000000000000000, -149.3052959529999839 ) ) ;
#22700 = ADVANCED_FACE ( 'NONE', ( #13100 ), #4067, .F. ) ;
#22701 = CARTESIAN_POINT ( 'NONE',  ( -30.02199999990000023, 40.89711431700000333, -146.3052959529999839 ) ) ;
#22702 = EDGE_LOOP ( 'NONE', ( #9575, #22867, #13308, #5458 ) ) ;
#22703 = LINE ( 'NONE', #20807, #5318 ) ;
#22704 = CARTESIAN_POINT ( 'NONE',  ( 8.900000000049999471, 39.46779253580000102, -148.7552959530000010 ) ) ;
#22705 = ORIENTED_EDGE ( 'NONE', *, *, #16572, .F. ) ;
#22706 = CARTESIAN_POINT ( 'NONE',  ( -14.45813593939999997, 41.09907220950000095, -141.6721478100000127 ) ) ;
#22707 = CARTESIAN_POINT ( 'NONE',  ( -25.52669956779758209, 32.98784426750318488, -146.4664506488380198 ) ) ;
#22708 = EDGE_LOOP ( 'NONE', ( #14393, #17360, #10799, #15494 ) ) ;
#22709 = DIRECTION ( 'NONE',  ( 0.000000000000000000, -1.000000000000000000, 0.000000000000000000 ) ) ;
#22710 = VERTEX_POINT ( 'NONE', #9635 ) ;
#22711 = DIRECTION ( 'NONE',  ( 2.257144641399999941E-12, 0.000000000000000000, 1.000000000000000000 ) ) ;
#22712 = PLANE ( 'NONE',  #11474 ) ;
#22713 = ORIENTED_EDGE ( 'NONE', *, *, #3995, .F. ) ;
#22714 = DIRECTION ( 'NONE',  ( 4.510774274160000731E-12, -1.321907670990000086E-13, 1.000000000000000000 ) ) ;
#22715 = VECTOR ( 'NONE', #21488, 1000.000000000000000 ) ;
#22716 = VERTEX_POINT ( 'NONE', #3956 ) ;
#22717 = LINE ( 'NONE', #19033, #10210 ) ;
#22718 = COLOUR_RGB ( '', 0.40784314, 0.44705882, 0.49803922) ;
#22719 = CARTESIAN_POINT ( 'NONE',  ( -4.499999999949999996, 31.50000000000000000, -150.0552959529999839 ) ) ;
#22720 = ORIENTED_EDGE ( 'NONE', *, *, #17299, .F. ) ;
#22721 = EDGE_LOOP ( 'NONE', ( #5399, #3328, #7338, #11734 ) ) ;
#22722 = CARTESIAN_POINT ( 'NONE',  ( 14.50000000010000001, 34.50000000000000000, -144.0552959529999839 ) ) ;
#22723 = CARTESIAN_POINT ( 'NONE',  ( -9.999999999969999109, 25.50000000000000000, -137.0552959530000123 ) ) ;
#22724 = LINE ( 'NONE', #2756, #21203 ) ;
#22725 = DIRECTION ( 'NONE',  ( -0.9846904924346531196, 0.1743118874569385135, 0.000000000000000000 ) ) ;
#22726 = ORIENTED_EDGE ( 'NONE', *, *, #4458, .T. ) ;
#22727 = DIRECTION ( 'NONE',  ( 1.000000000000000000, 0.000000000000000000, 0.000000000000000000 ) ) ;
#22728 = EDGE_CURVE ( 'NONE', #13760, #20840, #10680, .T. ) ;
#22729 = CARTESIAN_POINT ( 'NONE',  ( -8.971913342289999704, 37.83624783359999810, -148.2794752869999968 ) ) ;
#22730 = CIRCLE ( 'NONE', #9797, 2.000000000000001776 ) ;
#22731 = CARTESIAN_POINT ( 'NONE',  ( 25.89900052719454493, -18.65635984007525394, -150.0552959529999839 ) ) ;
#22732 = CARTESIAN_POINT ( 'NONE',  ( -4.499999999929999994, 42.50000000000000000, -138.0552959530000123 ) ) ;
#22733 = CARTESIAN_POINT ( 'NONE',  ( 15.50000000000000000, 39.50000000000000000, -136.0552959530000123 ) ) ;
#22734 = CARTESIAN_POINT ( 'NONE',  ( 23.89222110089999873, -31.59487100459999809, -146.0552959529999839 ) ) ;
#22735 = VECTOR ( 'NONE', #9230, 1000.000000000000000 ) ;
#22736 = VERTEX_POINT ( 'NONE', #22046 ) ;
#22737 = PLANE ( 'NONE',  #1225 ) ;
#22738 = CARTESIAN_POINT ( 'NONE',  ( 25.50000000000000000, 22.50000000000000000, -137.0552959530000123 ) ) ;
#22739 = ADVANCED_FACE ( 'NONE', ( #622 ), #11536, .T. ) ;
#22740 = CARTESIAN_POINT ( 'NONE',  ( -4.740745377972312546, 37.03357229754023194, -140.5852769423916300 ) ) ;
#22741 = DIRECTION ( 'NONE',  ( 3.994014902950000436E-29, -1.000000000000000000, 4.148443855749999753E-27 ) ) ;
#22742 = EDGE_LOOP ( 'NONE', ( #15603, #3086, #11174, #12641 ) ) ;
#22743 = CARTESIAN_POINT ( 'NONE',  ( -9.178237216079999428, 36.01795878010000251, -148.2568923610000127 ) ) ;
#22744 = PLANE ( 'NONE',  #12645 ) ;
#22745 = CARTESIAN_POINT ( 'NONE',  ( 5.961649142145938995, -3.109383212426971355, -150.0552959530000123 ) ) ;
#22746 = ORIENTED_EDGE ( 'NONE', *, *, #16800, .F. ) ;
#22747 = SURFACE_STYLE_FILL_AREA ( #15267 ) ;
#22748 = CIRCLE ( 'NONE', #9819, 8.000000000000000000 ) ;
#22749 = EDGE_CURVE ( 'NONE', #7827, #6123, #4347, .T. ) ;
#22750 = EDGE_CURVE ( 'NONE', #20332, #2028, #2177, .T. ) ;
#22751 = VECTOR ( 'NONE', #11898, 1000.000000000000000 ) ;
#22752 = CARTESIAN_POINT ( 'NONE',  ( -28.59946202390224101, 34.31616424881172378, -140.2812573677418015 ) ) ;
#22753 = FACE_OUTER_BOUND ( 'NONE', #21410, .T. ) ;
#22754 = VERTEX_POINT ( 'NONE', #7742 ) ;
#22755 = AXIS2_PLACEMENT_3D ( 'NONE', #171, #7644, #2082 ) ;
#22756 = CARTESIAN_POINT ( 'NONE',  ( -24.01715389780000010, 40.57582142210000598, -141.9832779239999923 ) ) ;
#22757 = ADVANCED_FACE ( 'NONE', ( #5844 ), #15125, .F. ) ;
#22758 = CARTESIAN_POINT ( 'NONE',  ( 8.500000000050000892, 37.00000000000000000, -148.0552959529999839 ) ) ;
#22759 = AXIS2_PLACEMENT_3D ( 'NONE', #20094, #17838, #1556 ) ;
#22760 = EDGE_CURVE ( 'NONE', #1347, #8811, #14514, .T. ) ;
#22761 = LINE ( 'NONE', #13838, #4442 ) ;
#22762 = DIRECTION ( 'NONE',  ( -1.000000000000000000, 5.094701932209999624E-24, 0.000000000000000000 ) ) ;
#22763 = CARTESIAN_POINT ( 'NONE',  ( -10.13646216689614299, 32.62416684293538083, -146.3387243813236296 ) ) ;
#22764 = CARTESIAN_POINT ( 'NONE',  ( 25.31684607440000079, 45.26810052429999587, -150.0552959529999839 ) ) ;
#22765 = CARTESIAN_POINT ( 'NONE',  ( -7.777479512046423515, 39.31680732581353510, -140.9495105956953864 ) ) ;
#22766 = EDGE_LOOP ( 'NONE', ( #9967, #21358, #13347, #22355 ) ) ;
#22767 = AXIS2_PLACEMENT_3D ( 'NONE', #14183, #17637, #1463 ) ;
#22768 = ADVANCED_FACE ( 'NONE', ( #5731, #12990 ), #20148, .F. ) ;
#22769 = VECTOR ( 'NONE', #20865, 1000.000000000000000 ) ;
#22770 = ORIENTED_EDGE ( 'NONE', *, *, #2362, .T. ) ;
#22771 = CARTESIAN_POINT ( 'NONE',  ( -7.069412601425229425, 33.52643604124185828, -143.7480921736344897 ) ) ;
#22772 = CARTESIAN_POINT ( 'NONE',  ( -27.26567793380000282, 36.96940380710000085, -148.4835048639999968 ) ) ;
#22773 = CARTESIAN_POINT ( 'NONE',  ( 23.17093239529999948, -15.44501179329999907, -143.5552959529999839 ) ) ;
#22774 = ADVANCED_FACE ( 'NONE', ( #3840 ), #2302, .T. ) ;
#22775 = VECTOR ( 'NONE', #4776, 1000.000000000000000 ) ;
#22776 = EDGE_LOOP ( 'NONE', ( #20430, #18508, #19904, #18381, #19174, #14860, #1397, #19225, #10952, #22680, #9049, #8951, #806, #21167, #7760 ) ) ;
#22777 = VECTOR ( 'NONE', #21892, 1000.000000000000000 ) ;
#22778 = DIRECTION ( 'NONE',  ( 1.000000000000000000, 0.000000000000000000, -2.262079412673755643E-12 ) ) ;
#22779 = CARTESIAN_POINT ( 'NONE',  ( -15.57786843150000067, 37.00666880280000726, -148.5521201120000114 ) ) ;
#22780 = EDGE_LOOP ( 'NONE', ( #12847, #22657, #10085, #19759 ) ) ;
#22781 = CARTESIAN_POINT ( 'NONE',  ( -21.80913741070000000, 38.74859698539999897, -147.9243209519999880 ) ) ;
#22782 = ADVANCED_FACE ( 'NONE', ( #20612 ), #9287, .F. ) ;
#22783 = CARTESIAN_POINT ( 'NONE',  ( -18.80116448531132889, 37.77574032756653821, -147.4754319351692402 ) ) ;
#22784 = EDGE_CURVE ( 'NONE', #23343, #4317, #5852, .T. ) ;
#22785 = CARTESIAN_POINT ( 'NONE',  ( -24.00000000000000000, 21.50000000000000000, -137.0552959530000123 ) ) ;
#22786 = LINE ( 'NONE', #4346, #15181 ) ;
#22787 = VECTOR ( 'NONE', #1403, 1000.000000000000000 ) ;
#22788 = EDGE_CURVE ( 'NONE', #12707, #6962, #15474, .T. ) ;
#22789 = DIRECTION ( 'NONE',  ( 0.7071067811865473507, -0.7071067811865476838, -1.591319668629389897E-12 ) ) ;
#22790 = VECTOR ( 'NONE', #22383, 1000.000000000000000 ) ;
#22791 = CARTESIAN_POINT ( 'NONE',  ( -24.10609388846707191, 35.33584289672160850, -147.6535802351943971 ) ) ;
#22792 = LINE ( 'NONE', #1377, #7842 ) ;
#22793 = VECTOR ( 'NONE', #13513, 1000.000000000000000 ) ;
#22794 = CIRCLE ( 'NONE', #21273, 3.000000000000000000 ) ;
#22795 = VECTOR ( 'NONE', #17730, 1000.000000000000000 ) ;
#22796 = CIRCLE ( 'NONE', #17859, 35.00000000000000000 ) ;
#22797 = VERTEX_POINT ( 'NONE', #11651 ) ;
#22798 = CARTESIAN_POINT ( 'NONE',  ( 16.61718498210000305, -18.75502267109999721, -142.5552959529999839 ) ) ;
#22799 = UNCERTAINTY_MEASURE_WITH_UNIT (LENGTH_MEASURE( 1.000000000000000082E-05 ), #18007, 'distance_accuracy_value', 'NONE');
#22800 = ORIENTED_EDGE ( 'NONE', *, *, #16227, .T. ) ;
#22801 = CARTESIAN_POINT ( 'NONE',  ( 1.172620240290000115, -63.19354141059999108, -145.5552959529999839 ) ) ;
#22802 = ORIENTED_EDGE ( 'NONE', *, *, #4600, .F. ) ;
#22803 = DIRECTION ( 'NONE',  ( 1.190078432789999897E-50, 1.000000000000000000, 0.000000000000000000 ) ) ;
#22804 = EDGE_LOOP ( 'NONE', ( #20461, #18908, #10171, #18065 ) ) ;
#22805 = CARTESIAN_POINT ( 'NONE',  ( -6.405315633307901990, -18.05400298756394406, -146.5552959530004387 ) ) ;
#22806 = VERTEX_POINT ( 'NONE', #973 ) ;
#22807 = ORIENTED_EDGE ( 'NONE', *, *, #18993, .T. ) ;
#22808 = CARTESIAN_POINT ( 'NONE',  ( -32.50000000000000000, 46.00000000000000000, -141.5552959529999839 ) ) ;
#22809 = CARTESIAN_POINT ( 'NONE',  ( -18.37691940361212062, 35.51168060177987940, -147.4900940512081888 ) ) ;
#22810 = CARTESIAN_POINT ( 'NONE',  ( -11.38486064716495960, 36.95668670071903961, -140.3965526140712257 ) ) ;
#22811 = CARTESIAN_POINT ( 'NONE',  ( 2.499999999879999990, -4.000000000000000000, -135.4552959529999896 ) ) ;
#22812 = VECTOR ( 'NONE', #12675, 1000.000000000000000 ) ;
#22813 = CIRCLE ( 'NONE', #4180, 6.000000000000001776 ) ;
#22814 = CARTESIAN_POINT ( 'NONE',  ( 16.33424841169999908, -31.58611763329999889, -148.0552959529999839 ) ) ;
#22815 = EDGE_CURVE ( 'NONE', #2118, #16530, #19989, .T. ) ;
#22816 = VECTOR ( 'NONE', #21025, 1000.000000000000000 ) ;
#22817 = CARTESIAN_POINT ( 'NONE',  ( 24.36715301250000110, -30.57462384669999977, -146.5552959529999839 ) ) ;
#22818 = ORIENTED_EDGE ( 'NONE', *, *, #20869, .T. ) ;
#22819 = PLANE ( 'NONE',  #5270 ) ;
#22820 = EDGE_CURVE ( 'NONE', #11337, #20932, #12133, .T. ) ;
#22821 = FACE_OUTER_BOUND ( 'NONE', #16228, .T. ) ;
#22822 = CARTESIAN_POINT ( 'NONE',  ( -9.334216945200001447, -17.19633444960000190, -146.5552959529999839 ) ) ;
#22823 = VERTEX_POINT ( 'NONE', #13693 ) ;
#22824 = PLANE ( 'NONE',  #11672 ) ;
#22825 = FACE_OUTER_BOUND ( 'NONE', #13798, .T. ) ;
#22826 = EDGE_LOOP ( 'NONE', ( #9309, #14224, #15189, #17580 ) ) ;
#22827 = CARTESIAN_POINT ( 'NONE',  ( 6.500000000030000002, 20.50000000000000000, -137.0552959530000123 ) ) ;
#22828 = AXIS2_PLACEMENT_3D ( 'NONE', #3576, #240, #7480 ) ;
#22829 = VECTOR ( 'NONE', #18256, 1000.000000000000000 ) ;
#22830 = ORIENTED_EDGE ( 'NONE', *, *, #17798, .F. ) ;
#22831 = CARTESIAN_POINT ( 'NONE',  ( -8.770737564319999180, -11.35481373070000011, -144.0552959529999839 ) ) ;
#22832 = DIRECTION ( 'NONE',  ( -1.000000000000000000, 2.312964634635743450E-15, 2.257453483404485639E-12 ) ) ;
#22833 = ORIENTED_EDGE ( 'NONE', *, *, #13015, .T. ) ;
#22834 = CARTESIAN_POINT ( 'NONE',  ( -14.68128999515341704, 37.84311035093374898, -139.6736120657584479 ) ) ;
#22835 = CARTESIAN_POINT ( 'NONE',  ( -26.51626171185139924, 36.02146533797493078, -139.7633415074477057 ) ) ;
#22836 = ORIENTED_EDGE ( 'NONE', *, *, #1267, .T. ) ;
#22837 = PRODUCT_DEFINITION_SHAPE ( 'NONE', 'NONE',  #23544 ) ;
#22838 = DIRECTION ( 'NONE',  ( 0.000000000000000000, 0.000000000000000000, 1.000000000000000000 ) ) ;
#22839 = ORIENTED_EDGE ( 'NONE', *, *, #22608, .T. ) ;
#22840 = LINE ( 'NONE', #4986, #18984 ) ;
#22841 = CARTESIAN_POINT ( 'NONE',  ( -8.734077015120000453, -11.22642389220000148, -146.5552959529999839 ) ) ;
#22842 = ORIENTED_EDGE ( 'NONE', *, *, #5183, .F. ) ;
#22843 = DIRECTION ( 'NONE',  ( 1.000000000000000000, 0.000000000000000000, 2.516505522483685870E-12 ) ) ;
#22844 = EDGE_CURVE ( 'NONE', #11330, #18727, #20965, .T. ) ;
#22845 = ORIENTED_EDGE ( 'NONE', *, *, #18534, .T. ) ;
#22846 = ADVANCED_FACE ( 'NONE', ( #11772 ), #17378, .T. ) ;
#22847 = CARTESIAN_POINT ( 'NONE',  ( 22.42591623494620023, -15.34961090601114542, -144.5552959529997281 ) ) ;
#22848 = DIRECTION ( 'NONE',  ( 2.257252162960000001E-12, 0.000000000000000000, 1.000000000000000000 ) ) ;
#22849 = EDGE_CURVE ( 'NONE', #12998, #6817, #19048, .T. ) ;
#22850 = ORIENTED_EDGE ( 'NONE', *, *, #23402, .T. ) ;
#22851 = AXIS2_PLACEMENT_3D ( 'NONE', #17648, #11475, #18753 ) ;
#22852 = CIRCLE ( 'NONE', #7251, 3.000000000000000000 ) ;
#22853 = VERTEX_POINT ( 'NONE', #17499 ) ;
#22854 = CYLINDRICAL_SURFACE ( 'NONE', #13145, 2.000000000000001776 ) ;
#22855 = CARTESIAN_POINT ( 'NONE',  ( -32.50000000000000000, 51.50000000000000000, -136.5552959530000123 ) ) ;
#22856 = CARTESIAN_POINT ( 'NONE',  ( -14.43541547443227557, 40.58553253640290137, -144.4623272911945833 ) ) ;
#22857 = DIRECTION ( 'NONE',  ( 0.000000000000000000, 0.000000000000000000, -1.000000000000000000 ) ) ;
#22858 = ORIENTED_EDGE ( 'NONE', *, *, #7497, .T. ) ;
#22859 =( NAMED_UNIT ( * ) SI_UNIT ( $, .STERADIAN. ) SOLID_ANGLE_UNIT ( ) );
#22860 = PLANE ( 'NONE',  #15022 ) ;
#22861 = EDGE_CURVE ( 'NONE', #5977, #16716, #9988, .T. ) ;
#22862 = CARTESIAN_POINT ( 'NONE',  ( 22.71475634692216161, -17.57808196999505768, -150.0552959529999839 ) ) ;
#22863 = DIRECTION ( 'NONE',  ( -0.7071067811865475727, -0.7071067811865475727, 0.000000000000000000 ) ) ;
#22864 = CARTESIAN_POINT ( 'NONE',  ( -11.59475511470959752, 36.93163239418914401, -139.6817994051292260 ) ) ;
#22865 = DIRECTION ( 'NONE',  ( -2.508215857230000030E-12, 0.000000000000000000, 1.000000000000000000 ) ) ;
#22866 = VECTOR ( 'NONE', #10601, 1000.000000000000000 ) ;
#22867 = ORIENTED_EDGE ( 'NONE', *, *, #13674, .T. ) ;
#22868 = AXIS2_PLACEMENT_3D ( 'NONE', #16372, #21736, #19938 ) ;
#22869 = DIRECTION ( 'NONE',  ( 0.000000000000000000, -1.000000000000000000, 0.000000000000000000 ) ) ;
#22870 = LINE ( 'NONE', #13697, #22775 ) ;
#22871 = CARTESIAN_POINT ( 'NONE',  ( 31.50000000000000000, 32.96379895120000469, -136.0552959530000123 ) ) ;
#22872 = CARTESIAN_POINT ( 'NONE',  ( 6.500000000149999124, 20.50000000000000000, -143.5552959529999839 ) ) ;
#22873 = LINE ( 'NONE', #15725, #11175 ) ;
#22874 = ORIENTED_EDGE ( 'NONE', *, *, #8018, .F. ) ;
#22875 = CARTESIAN_POINT ( 'NONE',  ( 12.50000000010000001, 16.89444872450000190, -147.5552959529999839 ) ) ;
#22876 = LINE ( 'NONE', #17392, #19880 ) ;
#22877 =( REPRESENTATION_RELATIONSHIP ('NONE','NONE', #7672, #15879 ) REPRESENTATION_RELATIONSHIP_WITH_TRANSFORMATION ( #7189 )SHAPE_REPRESENTATION_RELATIONSHIP( ) );
#22878 = CARTESIAN_POINT ( 'NONE',  ( -7.499999999969999109, 25.50000000000000000, -136.5552959530000123 ) ) ;
#22879 = EDGE_CURVE ( 'NONE', #8780, #10783, #11897, .T. ) ;
#22880 = ORIENTED_EDGE ( 'NONE', *, *, #20741, .T. ) ;
#22881 = FACE_OUTER_BOUND ( 'NONE', #11752, .T. ) ;
#22882 = DIRECTION ( 'NONE',  ( 1.000000000000000000, 0.000000000000000000, -2.259525899719999991E-12 ) ) ;
#22883 = AXIS2_PLACEMENT_3D ( 'NONE', #23533, #8528, #23065 ) ;
#22884 = CIRCLE ( 'NONE', #14532, 1.499999999999999556 ) ;
#22885 = DIRECTION ( 'NONE',  ( -0.9840552701943220404, 0.1778629393740580045, 0.000000000000000000 ) ) ;
#22886 = VERTEX_POINT ( 'NONE', #6551 ) ;
#22887 = AXIS2_PLACEMENT_3D ( 'NONE', #19534, #22984, #15606 ) ;
#22888 = CARTESIAN_POINT ( 'NONE',  ( -14.01657753872050094, 36.22806874875712424, -140.5479840251192059 ) ) ;
#22889 = DIRECTION ( 'NONE',  ( -1.000000000000000000, 0.000000000000000000, 2.258578509400000305E-12 ) ) ;
#22890 = EDGE_CURVE ( 'NONE', #6977, #7870, #22978, .T. ) ;
#22891 = CARTESIAN_POINT ( 'NONE',  ( -0.6176558849483760882, 18.08432684250963263, -150.0552959529999555 ) ) ;
#22892 = CARTESIAN_POINT ( 'NONE',  ( 8.401003265635759831, 38.49757205280096173, -142.0534435078293711 ) ) ;
#22893 = DIRECTION ( 'NONE',  ( 0.000000000000000000, -1.000000000000000000, 0.000000000000000000 ) ) ;
#22894 = CARTESIAN_POINT ( 'NONE',  ( 0.5374248537122892078, 25.07581004119178658, -150.0552959529999839 ) ) ;
#22895 = CARTESIAN_POINT ( 'NONE',  ( 4.579308732360918732, -33.90724429028959008, -150.0552959529999839 ) ) ;
#22896 = ORIENTED_EDGE ( 'NONE', *, *, #2143, .T. ) ;
#22897 = CARTESIAN_POINT ( 'NONE',  ( -22.00705883600000234, 37.05789963359999462, -148.1619053240000028 ) ) ;
#22898 = EDGE_CURVE ( 'NONE', #9410, #1301, #13450, .T. ) ;
#22899 = ORIENTED_EDGE ( 'NONE', *, *, #57, .T. ) ;
#22900 = CARTESIAN_POINT ( 'NONE',  ( -7.496535154942796986, 35.57088646773350860, -140.8259703478072993 ) ) ;
#22901 = CARTESIAN_POINT ( 'NONE',  ( -25.85824191589999899, -34.50000000000000000, -144.8157682190000060 ) ) ;
#22902 = DIRECTION ( 'NONE',  ( 2.257144641397284947E-12, -2.714724913984255017E-24, 1.000000000000000000 ) ) ;
#22903 = ORIENTED_EDGE ( 'NONE', *, *, #2191, .F. ) ;
#22904 = DIRECTION ( 'NONE',  ( 0.2024296638729825848, 0.9792968044389154247, -3.528679552389696828E-13 ) ) ;
#22905 = DIRECTION ( 'NONE',  ( 1.701177084980000217E-20, 4.426606872460000157E-37, 1.000000000000000000 ) ) ;
#22906 = ADVANCED_FACE ( 'NONE', ( #4770 ), #12017, .F. ) ;
#22907 = ORIENTED_EDGE ( 'NONE', *, *, #6208, .F. ) ;
#22908 = CARTESIAN_POINT ( 'NONE',  ( -20.93854596060227635, 37.74500530013531829, -147.9603137873362186 ) ) ;
#22909 = CARTESIAN_POINT ( 'NONE',  ( -17.27792307866062060, 37.67644708809300624, -140.6717186866207783 ) ) ;
#22910 = CARTESIAN_POINT ( 'NONE',  ( 4.128836048070000153, -25.17057797350000214, -148.5552959529999839 ) ) ;
#22911 = CARTESIAN_POINT ( 'NONE',  ( 7.831261784188757957, 35.65699296629090753, -146.1639638664211418 ) ) ;
#22912 = DIRECTION ( 'NONE',  ( 0.7071067811865473507, 0.7071067811865477948, -1.595945597898661113E-12 ) ) ;
#22913 = EDGE_CURVE ( 'NONE', #16792, #21766, #10228, .T. ) ;
#22914 = CARTESIAN_POINT ( 'NONE',  ( -24.95294881421506261, 33.96416018870619524, -145.8216992312312641 ) ) ;
#22915 = CARTESIAN_POINT ( 'NONE',  ( 6.000000000000001776, -3.699089422736518085, -150.0552959530000123 ) ) ;
#22916 = MECHANICAL_DESIGN_GEOMETRIC_PRESENTATION_REPRESENTATION (  '', ( #4296 ), #4670 ) ;
#22917 = EDGE_CURVE ( 'NONE', #7197, #7140, #6663, .T. ) ;
#22918 = FACE_OUTER_BOUND ( 'NONE', #9997, .T. ) ;
#22919 = CIRCLE ( 'NONE', #16443, 1.500000000000001332 ) ;
#22920 = ORIENTED_EDGE ( 'NONE', *, *, #8683, .T. ) ;
#22921 = DIRECTION ( 'NONE',  ( 0.000000000000000000, -1.000000000000000000, 0.000000000000000000 ) ) ;
#22922 = ORIENTED_EDGE ( 'NONE', *, *, #6753, .F. ) ;
#22923 = DIRECTION ( 'NONE',  ( 0.000000000000000000, 0.000000000000000000, 1.000000000000000000 ) ) ;
#22924 = EDGE_CURVE ( 'NONE', #10612, #384, #4886, .T. ) ;
#22925 = ORIENTED_EDGE ( 'NONE', *, *, #231, .F. ) ;
#22926 = DIRECTION ( 'NONE',  ( 0.000000000000000000, 0.000000000000000000, 1.000000000000000000 ) ) ;
#22927 = ADVANCED_FACE ( 'NONE', ( #4413 ), #9871, .T. ) ;
#22928 = ORIENTED_EDGE ( 'NONE', *, *, #22249, .F. ) ;
#22929 = LINE ( 'NONE', #15667, #14066 ) ;
#22930 = LINE ( 'NONE', #6847, #63 ) ;
#22931 = ORIENTED_EDGE ( 'NONE', *, *, #21610, .T. ) ;
#22932 = EDGE_CURVE ( 'NONE', #9140, #896, #13355, .T. ) ;
#22933 = ORIENTED_EDGE ( 'NONE', *, *, #14345, .T. ) ;
#22934 = CARTESIAN_POINT ( 'NONE',  ( -35.07300000000000040, 14.00000000000000000, -144.0552959529999839 ) ) ;
#22935 = EDGE_CURVE ( 'NONE', #16936, #7230, #6514, .T. ) ;
#22936 = CARTESIAN_POINT ( 'NONE',  ( -18.64600821080000159, 33.72696025770000006, -146.0724859999999978 ) ) ;
#22937 = CARTESIAN_POINT ( 'NONE',  ( -10.97748938910000049, 39.75689975739999937, -140.4868351200000234 ) ) ;
#22938 = PRODUCT_DEFINITION_FORMATION_WITH_SPECIFIED_SOURCE ( 'ANY', '', #18224, .NOT_KNOWN. ) ;
#22939 = DIRECTION ( 'NONE',  ( 0.000000000000000000, -1.000000000000000000, 0.000000000000000000 ) ) ;
#22940 = CARTESIAN_POINT ( 'NONE',  ( -7.801194085041059267, 32.45455882765661926, -143.7439339061524493 ) ) ;
#22941 = CARTESIAN_POINT ( 'NONE',  ( 6.500000000130000011, 16.50000000000000000, -150.5552959529999839 ) ) ;
#22942 = VERTEX_POINT ( 'NONE', #12253 ) ;
#22943 = CARTESIAN_POINT ( 'NONE',  ( -4.888913597060000171, -24.24628707910000003, -143.0552959529999839 ) ) ;
#22944 = CARTESIAN_POINT ( 'NONE',  ( -7.486908230310619139, 37.06387187510053138, -140.3212062627005707 ) ) ;
#22945 = DIRECTION ( 'NONE',  ( 2.839308199620000013E-14, 3.568879590630000244E-13, 1.000000000000000000 ) ) ;
#22946 = ORIENTED_EDGE ( 'NONE', *, *, #10115, .T. ) ;
#22947 = DIRECTION ( 'NONE',  ( 2.839308199620000013E-14, 3.568879590630000244E-13, 1.000000000000000000 ) ) ;
#22948 = VERTEX_POINT ( 'NONE', #14169 ) ;
#22949 = LINE ( 'NONE', #19132, #1832 ) ;
#22950 = LINE ( 'NONE', #9956, #3273 ) ;
#22951 = ORIENTED_EDGE ( 'NONE', *, *, #11865, .T. ) ;
#22952 = CARTESIAN_POINT ( 'NONE',  ( 8.400763094363121297, 38.49996446091597591, -146.0553226073556914 ) ) ;
#22953 = PLANE ( 'NONE',  #3499 ) ;
#22954 = ORIENTED_EDGE ( 'NONE', *, *, #10922, .F. ) ;
#22955 = CARTESIAN_POINT ( 'NONE',  ( -15.48617276601169834, 40.96818823142278632, -144.3825155029135772 ) ) ;
#22956 = EDGE_CURVE ( 'NONE', #1104, #13536, #5007, .T. ) ;
#22957 = CARTESIAN_POINT ( 'NONE',  ( -26.51312621108908019, 36.10278884006311273, -140.1473911447703529 ) ) ;
#22958 = ORIENTED_EDGE ( 'NONE', *, *, #8320, .T. ) ;
#22959 = ORIENTED_EDGE ( 'NONE', *, *, #11384, .T. ) ;
#22960 = CARTESIAN_POINT ( 'NONE',  ( -11.48759298129999884, 37.74537190000000209, -140.3874188149999895 ) ) ;
#22961 = B_SPLINE_CURVE_WITH_KNOTS ( 'NONE', 3,
 ( #17691, #3535, #18164, #1877, #21748, #19950, #14595, #16265, #3650, #12560, #5547, #19838, #9101, #16384, #23401, #15899, #12439, #19714, #19599, #14358, #5437, #1759, #7333, #91, #8981, #21863, #12794, #5079, #21507, #23521, #14482, #1528, #7218, #12681, #23289, #20067, #17805, #3764, #8624, #3294, #8749, #1399, #23165, #6860, #10652, #14125, #1648, #21393, #12323, #8869, #10526, #21628, #16028, #6981, #14243, #5190, #16147, #3996, #11228, #2001, #22431, #18395, #20194, #18746, #311, #18502, #9441, #2221, #12911, #5887, #433, #20414, #7671, #15172, #2456, #20533, #16719, #6004, #2344, #5655, #15051, #21969, #14941, #22203, #13144, #16841, #11468, #4106, #6127, #9678, #13258, #22087, #7786, #16954, #20651, #9568, #11344, #7552, #4233, #11007, #13383, #553, #18629, #22311, #660, #3890, #7893, #5775, #2104, #18290, #9221, #16489 ),
 .UNSPECIFIED., .F., .F.,
 ( 4, 2, 1, 2, 2, 2, 1, 1, 2, 2, 2, 2, 1, 1, 1, 2, 2, 2, 2, 2, 1, 2, 2, 2, 2, 1, 2, 2, 2, 1, 2, 2, 2, 2, 2, 1, 2, 2, 2, 1, 1, 2, 2, 2, 2, 1, 1, 2, 2, 2, 2, 1, 1, 1, 2, 2, 2, 1, 1, 2, 2, 2, 1, 2, 2, 4 ),
 ( 0.000000000000000000, 0.03125000000007426698, 0.04687500000011055046, 0.05468750000012817525, 0.06250000000014580004, 0.09375000000021557756, 0.1093750000002510908, 0.1171875000002707279, 0.1210937500002829403, 0.1250000000002951528, 0.1562500000004152234, 0.1718750000004748146, 0.1796875000005022649, 0.1835937500005136447, 0.1855468750005199452, 0.1865234375005227485, 0.1875000000005255518, 0.2187500000006049050, 0.2343750000006437628, 0.2421875000006631917, 0.2460937500006700751, 0.2480468750006724898, 0.2500000000006749046, 0.2812500000006796230, 0.2968750000006838974, 0.3046875000006860068, 0.3085937500006871170, 0.3125000000006881717, 0.3437500000006842860, 0.3593750000006820100, 0.3671875000006808443, 0.3750000000006796785, 0.5000000000007456258, 0.5625000000007787104, 0.5937500000007961409, 0.6093750000008081313, 0.6171875000008142376, 0.6250000000008202328, 0.6562500000008438805, 0.6718750000008558709, 0.6796875000008618661, 0.6835937500008635315, 0.6875000000008651968, 0.7187500000009028334, 0.7343750000009242607, 0.7421875000009376944, 0.7460937500009454659, 0.7480468750009519052, 0.7500000000009582335, 0.7812500000010785817, 0.7968750000011431966, 0.8046875000011735057, 0.8085937500011912693, 0.8105468750012013723, 0.8115234375011972645, 0.8125000000011932677, 0.8437500000010063061, 0.8593750000009123813, 0.8671875000008619772, 0.8710937500008353318, 0.8750000000008085754, 0.9062500000006017409, 0.9218750000005005996, 0.9296875000004484191, 0.9375000000003962386, 1.000000000000000000 ),
 .UNSPECIFIED. ) ;
#22962 = CARTESIAN_POINT ( 'NONE',  ( 13.68320006080000084, -20.50000000000000000, -138.5552959529999839 ) ) ;
#22963 = ORIENTED_EDGE ( 'NONE', *, *, #4725, .T. ) ;
#22964 = LINE ( 'NONE', #17605, #13289 ) ;
#22965 = CARTESIAN_POINT ( 'NONE',  ( -34.35824191590000254, -34.50000000000000000, -141.0657682190000060 ) ) ;
#22966 = CARTESIAN_POINT ( 'NONE',  ( -25.44349950029999974, 35.21826511839999796, -139.9516901549999943 ) ) ;
#22967 = AXIS2_PLACEMENT_3D ( 'NONE', #16944, #11811, #9430 ) ;
#22968 = ORIENTED_EDGE ( 'NONE', *, *, #2016, .F. ) ;
#22969 = CARTESIAN_POINT ( 'NONE',  ( 7.500000000000000000, -3.500000000000000000, -150.0552959529999839 ) ) ;
#22970 = DIRECTION ( 'NONE',  ( 4.500711553433139826E-12, 0.000000000000000000, 1.000000000000000000 ) ) ;
#22971 = CARTESIAN_POINT ( 'NONE',  ( -13.60171424471084478, 38.61389101324630246, -140.5757119291933748 ) ) ;
#22972 = PLANE ( 'NONE',  #23164 ) ;
#22973 = ORIENTED_EDGE ( 'NONE', *, *, #14411, .T. ) ;
#22974 = CARTESIAN_POINT ( 'NONE',  ( -32.50000000000000000, 1.000000000000000000, -137.0552959530000123 ) ) ;
#22975 = DIRECTION ( 'NONE',  ( 1.000000000000000000, 0.000000000000000000, 0.000000000000000000 ) ) ;
#22976 = FACE_OUTER_BOUND ( 'NONE', #12338, .T. ) ;
#22977 = CARTESIAN_POINT ( 'NONE',  ( 23.00000000000000000, 19.50000000000000000, -150.0552959529999839 ) ) ;
#22978 = LINE ( 'NONE', #17265, #17544 ) ;
#22979 = EDGE_CURVE ( 'NONE', #9016, #12276, #12722, .T. ) ;
#22980 = CARTESIAN_POINT ( 'NONE',  ( 16.13369214839999799, 51.50000000000000000, -136.0552959530000123 ) ) ;
#22981 = VERTEX_POINT ( 'NONE', #3692 ) ;
#22982 = CARTESIAN_POINT ( 'NONE',  ( -16.81794493339610241, 37.02435727936596521, -140.5111119823619958 ) ) ;
#22983 = PLANE ( 'NONE',  #22019 ) ;
#22984 = DIRECTION ( 'NONE',  ( -0.1465035852930155202, -0.9892101392001055871, 4.561368942930487546E-14 ) ) ;
#22985 = DIRECTION ( 'NONE',  ( 2.507771768019999718E-12, 1.592654864209999947E-17, -1.000000000000000000 ) ) ;
#22986 = FACE_OUTER_BOUND ( 'NONE', #18459, .T. ) ;
#22987 = ORIENTED_EDGE ( 'NONE', *, *, #13531, .T. ) ;
#22988 = FACE_OUTER_BOUND ( 'NONE', #4864, .T. ) ;
#22989 = DIRECTION ( 'NONE',  ( -0.7071067811865474617, 0.7071067811865476838, 1.595020412044806951E-12 ) ) ;
#22990 = CARTESIAN_POINT ( 'NONE',  ( -25.46021907539999773, 33.59345108530000346, -146.1038275270000213 ) ) ;
#22991 = ORIENTED_EDGE ( 'NONE', *, *, #8408, .T. ) ;
#22992 = CARTESIAN_POINT ( 'NONE',  ( -28.03429568396224170, 32.40695676819103710, -144.4586890253826255 ) ) ;
#22993 = DIRECTION ( 'NONE',  ( 2.257171095940000041E-12, 1.003664318210000046E-28, 1.000000000000000000 ) ) ;
#22994 = ORIENTED_EDGE ( 'NONE', *, *, #1982, .T. ) ;
#22995 = CARTESIAN_POINT ( 'NONE',  ( -24.21925763020469802, 40.64313348517629265, -144.4529654621569819 ) ) ;
#22996 = CARTESIAN_POINT ( 'NONE',  ( -20.60824191589999899, -4.000000000000000000, -145.5657682190000060 ) ) ;
#22997 = FACE_OUTER_BOUND ( 'NONE', #16583, .T. ) ;
#22998 = CARTESIAN_POINT ( 'NONE',  ( 8.212030648970713997, 38.47214394625672185, -142.0347430633063937 ) ) ;
#22999 = VECTOR ( 'NONE', #2033, 1000.000000000000000 ) ;
#23000 = ORIENTED_EDGE ( 'NONE', *, *, #9181, .F. ) ;
#23001 = CARTESIAN_POINT ( 'NONE',  ( -5.932764524189999555, 37.76833845600000217, -147.9772051180000005 ) ) ;
#23002 = DIRECTION ( 'NONE',  ( 1.701177084980000217E-20, 4.426606872460000157E-37, 1.000000000000000000 ) ) ;
#23003 = CARTESIAN_POINT ( 'NONE',  ( -9.092633533251282429, 40.57158656394992846, -143.6010347923813129 ) ) ;
#23004 = CARTESIAN_POINT ( 'NONE',  ( -16.35051508389999597, -1.500000000000000000, -147.0118839079999873 ) ) ;
#23005 = EDGE_CURVE ( 'NONE', #8394, #21209, #21794, .T. ) ;
#23006 = VECTOR ( 'NONE', #19833, 1000.000000000000114 ) ;
#23007 = ORIENTED_EDGE ( 'NONE', *, *, #9511, .F. ) ;
#23008 = EDGE_CURVE ( 'NONE', #16273, #2045, #21550, .T. ) ;
#23009 = SURFACE_STYLE_USAGE ( .BOTH. , #17411 ) ;
#23010 = B_SPLINE_CURVE_WITH_KNOTS ( 'NONE', 3,
 ( #17193, #22232, #6247, #12828, #13496, #20101, #11153, #3803, #17557, #20896, #15527, #21248, #1273, #6490, #17427, #8604, #22915, #19100 ),
 .UNSPECIFIED., .F., .F.,
 ( 4, 2, 2, 2, 2, 2, 2, 2, 4 ),
 ( 0.000000000000000000, 0.1249999999999998612, 0.2499999999999997224, 0.3749999999999995559, 0.4999999999999992228, 0.6249999999999994449, 0.7499999999999995559, 0.8749999999999997780, 1.000000000000000000 ),
 .UNSPECIFIED. ) ;
#23011 = ORIENTED_EDGE ( 'NONE', *, *, #17652, .T. ) ;
#23012 = CARTESIAN_POINT ( 'NONE',  ( -7.206173031900359405, 35.38491483727327847, -147.9515367338636054 ) ) ;
#23013 = CARTESIAN_POINT ( 'NONE',  ( -27.06022691649999956, 38.83733237969999408, -148.2479545119999784 ) ) ;
#23014 = CARTESIAN_POINT ( 'NONE',  ( 4.500000000009999113, -3.500000000000000000, -136.0552959530000123 ) ) ;
#23015 = ORIENTED_EDGE ( 'NONE', *, *, #10655, .T. ) ;
#23016 = DIRECTION ( 'NONE',  ( 1.000000000000000000, 0.000000000000000000, -1.526556658859589738E-13 ) ) ;
#23017 = LINE ( 'NONE', #21238, #22053 ) ;
#23018 = VECTOR ( 'NONE', #11451, 1000.000000000000000 ) ;
#23019 = CIRCLE ( 'NONE', #13503, 2.999999999999999112 ) ;
#23020 = VERTEX_POINT ( 'NONE', #14047 ) ;
#23021 = DIRECTION ( 'NONE',  ( -0.7071067811865484609, 0.7071067811865466846, -1.776356839400247234E-12 ) ) ;
#23022 = CARTESIAN_POINT ( 'NONE',  ( -18.65864117670379585, 40.55340188292282022, -145.9561081538003862 ) ) ;
#23023 = DIRECTION ( 'NONE',  ( -0.6459422414661291079, 0.7633862853691523176, -2.245315045000450442E-12 ) ) ;
#23024 = DIRECTION ( 'NONE',  ( 2.257157423930000049E-12, 0.000000000000000000, 1.000000000000000000 ) ) ;
#23025 = ADVANCED_FACE ( 'NONE', ( #1687 ), #15828, .F. ) ;
#23026 = DIRECTION ( 'NONE',  ( -1.000000000000000000, 0.000000000000000000, 0.000000000000000000 ) ) ;
#23027 = CARTESIAN_POINT ( 'NONE',  ( -17.52779041586177300, 36.93962571632795999, -139.7364823516871581 ) ) ;
#23028 = FACE_OUTER_BOUND ( 'NONE', #13223, .T. ) ;
#23029 = CARTESIAN_POINT ( 'NONE',  ( -12.56920363940049512, 37.00563451942266369, -148.6543378380284821 ) ) ;
#23030 = ORIENTED_EDGE ( 'NONE', *, *, #5060, .F. ) ;
#23031 = VECTOR ( 'NONE', #14742, 1000.000000000000000 ) ;
#23032 = CARTESIAN_POINT ( 'NONE',  ( 16.13369214859999801, 50.50000000000000000, -136.0552959530000123 ) ) ;
#23033 = EDGE_CURVE ( 'NONE', #16183, #17995, #14222, .T. ) ;
#23034 = VECTOR ( 'NONE', #13361, 1000.000000000000000 ) ;
#23035 = PRODUCT_DEFINITION_CONTEXT ( 'detailed design', #19210, 'design' ) ;
#23036 = ORIENTED_EDGE ( 'NONE', *, *, #18009, .F. ) ;
#23037 = ORIENTED_EDGE ( 'NONE', *, *, #14777, .F. ) ;
#23038 = DIRECTION ( 'NONE',  ( 0.000000000000000000, 2.256988247090000272E-12, 1.000000000000000000 ) ) ;
#23039 = CARTESIAN_POINT ( 'NONE',  ( -28.81387671664944250, 37.02484288695405468, -140.6184821045081037 ) ) ;
#23040 = ORIENTED_EDGE ( 'NONE', *, *, #18531, .F. ) ;
#23041 = ORIENTED_EDGE ( 'NONE', *, *, #14437, .T. ) ;
#23042 = DIRECTION ( 'NONE',  ( 0.000000000000000000, 1.000000000000000000, 0.000000000000000000 ) ) ;
#23043 = EDGE_CURVE ( 'NONE', #22550, #19256, #21675, .T. ) ;
#23044 = DIRECTION ( 'NONE',  ( 0.000000000000000000, 1.000000000000000000, 0.000000000000000000 ) ) ;
#23045 = CARTESIAN_POINT ( 'NONE',  ( -11.79464594726566062, 38.67573169081060058, -148.1300312029912050 ) ) ;
#23046 = CARTESIAN_POINT ( 'NONE',  ( 15.50000000000000000, 39.50000000000000000, -150.0552959529999839 ) ) ;
#23047 =( BOUNDED_CURVE ( )  B_SPLINE_CURVE ( 5, ( #11795, #13236, #7993, #15276, #20512, #22642 ),
 .UNSPECIFIED., .F., .F. ) 
 B_SPLINE_CURVE_WITH_KNOTS ( ( 6, 6 ),
 ( 0.000000000000000000, 1.570796326654103181 ),
 .UNSPECIFIED. ) 
 CURVE ( )  GEOMETRIC_REPRESENTATION_ITEM ( )  RATIONAL_B_SPLINE_CURVE ( ( 1.000000000000000000, 0.6000000000358791663, 0.4000000000358792107, 0.3000000000269094080, 0.2500000000179396498, 0.2500000000000000555 ) ) 
 REPRESENTATION_ITEM ( '' )  );
#23048 = CARTESIAN_POINT ( 'NONE',  ( -7.572469997258134633, 37.05365869149841984, -139.6601318950651773 ) ) ;
#23049 = VERTEX_POINT ( 'NONE', #14281 ) ;
#23050 = DIRECTION ( 'NONE',  ( 1.000000000000000000, 0.000000000000000000, 0.000000000000000000 ) ) ;
#23051 = AXIS2_PLACEMENT_3D ( 'NONE', #15115, #22261, #13329 ) ;
#23052 = EDGE_CURVE ( 'NONE', #22250, #18790, #23211, .T. ) ;
#23053 = CARTESIAN_POINT ( 'NONE',  ( 6.000000000010001777, -3.696349540849364512, -136.0552959530033945 ) ) ;
#23054 = EDGE_CURVE ( 'NONE', #17215, #15634, #3459, .T. ) ;
#23055 = DIRECTION ( 'NONE',  ( 0.000000000000000000, -1.000000000000000000, 3.568879590630000244E-13 ) ) ;
#23056 = ORIENTED_EDGE ( 'NONE', *, *, #17057, .T. ) ;
#23057 = EDGE_CURVE ( 'NONE', #21227, #10304, #19638, .T. ) ;
#23058 = EDGE_CURVE ( 'NONE', #7250, #10198, #17856, .T. ) ;
#23059 = DIRECTION ( 'NONE',  ( -2.257144641399999941E-12, 0.000000000000000000, -1.000000000000000000 ) ) ;
#23060 = ORIENTED_EDGE ( 'NONE', *, *, #21833, .F. ) ;
#23061 = CARTESIAN_POINT ( 'NONE',  ( -20.26899604980000191, 40.93030953040000242, -143.7497896410000067 ) ) ;
#23062 = CARTESIAN_POINT ( 'NONE',  ( 31.50000000000000000, 0.000000000000000000, -136.0552959530000123 ) ) ;
#23063 = ORIENTED_EDGE ( 'NONE', *, *, #1180, .F. ) ;
#23064 = CARTESIAN_POINT ( 'NONE',  ( 7.683200060759999950, -21.50000000000000000, -148.5552959529999839 ) ) ;
#23065 = DIRECTION ( 'NONE',  ( 0.000000000000000000, 0.000000000000000000, 1.000000000000000000 ) ) ;
#23066 = EDGE_LOOP ( 'NONE', ( #8238, #7096, #9715, #11817 ) ) ;
#23067 = CARTESIAN_POINT ( 'NONE',  ( -14.79658270967934008, 39.12156175677914405, -141.0283858338752339 ) ) ;
#23068 = CIRCLE ( 'NONE', #16600, 1.499999999999999556 ) ;
#23069 = CARTESIAN_POINT ( 'NONE',  ( -26.61707828802655484, 36.92896776167479089, -139.7487649555727103 ) ) ;
#23070 = ORIENTED_EDGE ( 'NONE', *, *, #1412, .T. ) ;
#23071 = DIRECTION ( 'NONE',  ( 0.000000000000000000, 0.000000000000000000, 1.000000000000000000 ) ) ;
#23072 = VERTEX_POINT ( 'NONE', #16307 ) ;
#23073 = CARTESIAN_POINT ( 'NONE',  ( -12.76385253890000016, 37.02886902030000016, -147.6186336929999925 ) ) ;
#23074 = DIRECTION ( 'NONE',  ( 1.000000000000000000, 0.000000000000000000, -1.526556658859589738E-13 ) ) ;
#23075 = ORIENTED_EDGE ( 'NONE', *, *, #1525, .F. ) ;
#23076 = DIRECTION ( 'NONE',  ( 1.000000000000000000, 0.000000000000000000, -4.430318231639999944E-12 ) ) ;
#23077 = EDGE_CURVE ( 'NONE', #4115, #21983, #8792, .T. ) ;
#23078 = CARTESIAN_POINT ( 'NONE',  ( -32.50000000000000000, 26.00000000000000000, -146.5552959529999839 ) ) ;
#23079 = PLANE ( 'NONE',  #18554 ) ;
#23080 = AXIS2_PLACEMENT_3D ( 'NONE', #8843, #3975, #15029 ) ;
#23081 = EDGE_CURVE ( 'NONE', #10244, #16283, #7138, .T. ) ;
#23082 = EDGE_CURVE ( 'NONE', #21713, #15726, #3578, .T. ) ;
#23083 = VERTEX_POINT ( 'NONE', #1801 ) ;
#23084 = CARTESIAN_POINT ( 'NONE',  ( -21.35824191589185972, -32.00000000000000000, -149.4708568729758724 ) ) ;
#23085 = PLANE ( 'NONE',  #21105 ) ;
#23086 = CARTESIAN_POINT ( 'NONE',  ( -13.90907534077411434, 39.72570884558322746, -140.3685967658352638 ) ) ;
#23087 = CYLINDRICAL_SURFACE ( 'NONE', #16323, 1.000000000000001332 ) ;
#23088 = ORIENTED_EDGE ( 'NONE', *, *, #9952, .T. ) ;
#23089 = LINE ( 'NONE', #18925, #5618 ) ;
#23090 = CARTESIAN_POINT ( 'NONE',  ( -7.520331543250000195, 50.50000000000000000, -136.0552959530000123 ) ) ;
#23091 = PLANE ( 'NONE',  #7239 ) ;
#23092 = CARTESIAN_POINT ( 'NONE',  ( -28.81387671665526895, 37.02484288695334413, -140.6184821045066826 ) ) ;
#23093 = CARTESIAN_POINT ( 'NONE',  ( 12.50000000010000001, 20.50000000000000000, -150.5552959529999839 ) ) ;
#23094 = EDGE_LOOP ( 'NONE', ( #12126, #22946, #8992, #16765 ) ) ;
#23095 = CARTESIAN_POINT ( 'NONE',  ( -16.26754611222665048, 35.58143005778827472, -140.5099932849695961 ) ) ;
#23096 = CIRCLE ( 'NONE', #5612, 1.500000000000001332 ) ;
#23097 = LINE ( 'NONE', #8674, #20878 ) ;
#23098 =( GEOMETRIC_REPRESENTATION_CONTEXT ( 3 ) GLOBAL_UNCERTAINTY_ASSIGNED_CONTEXT ( ( #9203 ) ) GLOBAL_UNIT_ASSIGNED_CONTEXT ( ( #21078, #4764, #22859 ) ) REPRESENTATION_CONTEXT ( 'NONE', 'WORKASPACE' ) );
#23099 = DIRECTION ( 'NONE',  ( -0.07970438983373200059, -0.9968185442904001770, 8.265980492683321082E-13 ) ) ;
#23100 = PLANE ( 'NONE',  #11088 ) ;
#23101 = LINE ( 'NONE', #6791, #552 ) ;
#23102 = ORIENTED_EDGE ( 'NONE', *, *, #9679, .T. ) ;
#23103 = DIRECTION ( 'NONE',  ( 0.6183952767652367566, -0.7858672163123019416, -2.891205793294677010E-12 ) ) ;
#23104 = CARTESIAN_POINT ( 'NONE',  ( -25.91744746520000220, 33.58572460659999592, -142.1592104600000255 ) ) ;
#23105 = VERTEX_POINT ( 'NONE', #14 ) ;
#23106 = EDGE_CURVE ( 'NONE', #9000, #20464, #6971, .T. ) ;
#23107 = ADVANCED_FACE ( 'NONE', ( #357 ), #7598, .T. ) ;
#23108 = DIRECTION ( 'NONE',  ( -1.000000000000000000, 0.000000000000000000, 2.257144641399999941E-12 ) ) ;
#23109 = DIRECTION ( 'NONE',  ( -0.9847555042252370550, 0.1739442350240419932, 1.062521554950256121E-14 ) ) ;
#23110 = ORIENTED_EDGE ( 'NONE', *, *, #11564, .T. ) ;
#23111 = DIRECTION ( 'NONE',  ( -1.000000000000000000, 0.000000000000000000, 2.257221436789999912E-12 ) ) ;
#23112 = VECTOR ( 'NONE', #16674, 1000.000000000000000 ) ;
#23113 = DIRECTION ( 'NONE',  ( -4.510774274160000731E-12, 1.321907670990000086E-13, -1.000000000000000000 ) ) ;
#23114 = AXIS2_PLACEMENT_3D ( 'NONE', #21759, #6866, #14135 ) ;
#23115 = FACE_BOUND ( 'NONE', #2097, .T. ) ;
#23116 = CARTESIAN_POINT ( 'NONE',  ( 7.286767612010325301, 37.88214748707077462, -141.7161147874617768 ) ) ;
#23117 = VERTEX_POINT ( 'NONE', #13187 ) ;
#23118 = CARTESIAN_POINT ( 'NONE',  ( -10.01829490536019662, 32.29821814703051075, -144.2706886520148828 ) ) ;
#23119 = DIRECTION ( 'NONE',  ( -2.257171095940000041E-12, 0.000000000000000000, -1.000000000000000000 ) ) ;
#23120 = CARTESIAN_POINT ( 'NONE',  ( -9.674592407298980845, 39.37273218293604060, -147.1879168912154228 ) ) ;
#23121 = PLANE ( 'NONE',  #9528 ) ;
#23122 = ORIENTED_EDGE ( 'NONE', *, *, #21351, .T. ) ;
#23123 = LINE ( 'NONE', #3144, #9529 ) ;
#23124 =( NAMED_UNIT ( * ) PLANE_ANGLE_UNIT ( ) SI_UNIT ( $, .RADIAN. ) );
#23125 = VERTEX_POINT ( 'NONE', #7482 ) ;
#23126 = CARTESIAN_POINT ( 'NONE',  ( -8.008464111606381053, 33.29536412533623491, -142.0809313903132249 ) ) ;
#23127 = LINE ( 'NONE', #14315, #96 ) ;
#23128 = CARTESIAN_POINT ( 'NONE',  ( 6.000000000140000012, 36.50000000000000000, -146.5552959529999839 ) ) ;
#23129 = AXIS2_PLACEMENT_3D ( 'NONE', #22083, #877, #15376 ) ;
#23130 = AXIS2_PLACEMENT_3D ( 'NONE', #10051, #19229, #21151 ) ;
#23131 = ORIENTED_EDGE ( 'NONE', *, *, #9339, .F. ) ;
#23132 = CARTESIAN_POINT ( 'NONE',  ( 8.500000000060001781, 37.00000000000000000, -144.0552959529999839 ) ) ;
#23133 = DIRECTION ( 'NONE',  ( 0.000000000000000000, 0.000000000000000000, -1.000000000000000000 ) ) ;
#23134 = VECTOR ( 'NONE', #5819, 1000.000000000000114 ) ;
#23135 = ORIENTED_EDGE ( 'NONE', *, *, #4898, .T. ) ;
#23136 = CARTESIAN_POINT ( 'NONE',  ( -17.53569647200000148, 40.68917497039999631, -144.4123951040000122 ) ) ;
#23137 = EDGE_CURVE ( 'NONE', #12827, #18274, #9264, .T. ) ;
#23138 = CIRCLE ( 'NONE', #6019, 2.500000000000002220 ) ;
#23139 = LINE ( 'NONE', #21366, #20498 ) ;
#23140 = DIRECTION ( 'NONE',  ( 2.257144641399999941E-12, -4.009147065140000298E-51, 1.000000000000000000 ) ) ;
#23141 = EDGE_CURVE ( 'NONE', #7563, #19876, #9559, .T. ) ;
#23142 = CARTESIAN_POINT ( 'NONE',  ( -33.50000000000000000, 28.00000000000000000, -146.5552959529999839 ) ) ;
#23143 = ADVANCED_BREP_SHAPE_REPRESENTATION ( '', ( #20181, #5025 ), #10730 ) ;
#23144 = CARTESIAN_POINT ( 'NONE',  ( 17.58326321919999558, -18.99156222550000095, -147.0552959529999839 ) ) ;
#23145 = CARTESIAN_POINT ( 'NONE',  ( -9.923478264230000789, -23.29931827799999766, -144.0552959529999839 ) ) ;
#23146 = PLANE ( 'NONE',  #18488 ) ;
#23147 = CARTESIAN_POINT ( 'NONE',  ( -34.50000000000000000, 26.00000000000000000, -148.5552959529999839 ) ) ;
#23148 = AXIS2_PLACEMENT_3D ( 'NONE', #4993, #13676, #19151 ) ;
#23149 = ORIENTED_EDGE ( 'NONE', *, *, #17578, .F. ) ;
#23150 = DIRECTION ( 'NONE',  ( 1.000000000000000000, 0.000000000000000000, -2.257453483404484831E-12 ) ) ;
#23151 = ORIENTED_EDGE ( 'NONE', *, *, #5380, .F. ) ;
#23152 = ORIENTED_EDGE ( 'NONE', *, *, #15508, .T. ) ;
#23153 = CARTESIAN_POINT ( 'NONE',  ( -31.50000000000000000, -14.25000000000000000, -150.0552959529999839 ) ) ;
#23154 = CARTESIAN_POINT ( 'NONE',  ( -28.47499893024826889, 37.06529344307018192, -140.4421442387167360 ) ) ;
#23155 = ORIENTED_EDGE ( 'NONE', *, *, #12726, .T. ) ;
#23156 = ORIENTED_EDGE ( 'NONE', *, *, #17217, .T. ) ;
#23157 = CARTESIAN_POINT ( 'NONE',  ( -4.500067286957687429, 22.89748944254456831, -150.0552959529999839 ) ) ;
#23158 = CARTESIAN_POINT ( 'NONE',  ( -8.514310886080000529, 36.94123471670000214, -140.1199228270000106 ) ) ;
#23159 = CARTESIAN_POINT ( 'NONE',  ( -9.282104535860000283, -16.71402168319999859, -145.5552959529999839 ) ) ;
#23160 = LINE ( 'NONE', #17927, #6499 ) ;
#23161 = CARTESIAN_POINT ( 'NONE',  ( -7.363485702945446576, 35.16406626390504897, -139.8948755779048270 ) ) ;
#23162 = VECTOR ( 'NONE', #20628, 1000.000000000000000 ) ;
#23163 = VERTEX_POINT ( 'NONE', #16644 ) ;
#23164 = AXIS2_PLACEMENT_3D ( 'NONE', #6197, #17016, #22725 ) ;
#23165 = CARTESIAN_POINT ( 'NONE',  ( 9.713232388825044694, 36.11785251390046625, -141.7161147870856155 ) ) ;
#23166 = EDGE_CURVE ( 'NONE', #10162, #13656, #16429, .T. ) ;
#23167 = AXIS2_PLACEMENT_3D ( 'NONE', #10325, #15923, #10203 ) ;
#23168 = FACE_OUTER_BOUND ( 'NONE', #1787, .T. ) ;
#23169 = AXIS2_PLACEMENT_3D ( 'NONE', #15872, #21368, #23490 ) ;
#23170 = AXIS2_PLACEMENT_3D ( 'NONE', #3094, #19511, #17359 ) ;
#23171 = DIRECTION ( 'NONE',  ( -1.211690350420779919E-27, -2.765629237169220318E-27, 1.000000000000000000 ) ) ;
#23172 = ORIENTED_EDGE ( 'NONE', *, *, #17732, .T. ) ;
#23173 = CARTESIAN_POINT ( 'NONE',  ( -9.334216945200001447, -17.19633444960000190, -146.5552959529999839 ) ) ;
#23174 = ORIENTED_EDGE ( 'NONE', *, *, #5961, .T. ) ;
#23175 = DIRECTION ( 'NONE',  ( 0.000000000000000000, -1.000000000000000000, 0.000000000000000000 ) ) ;
#23176 = DIRECTION ( 'NONE',  ( -0.9949850929136110356, 0.1000233216789610247, -7.446425804567087094E-15 ) ) ;
#23177 = VERTEX_POINT ( 'NONE', #11275 ) ;
#23178 = CARTESIAN_POINT ( 'NONE',  ( 8.500000000070000894, 37.00000000000000000, -138.5552959529999839 ) ) ;
#23179 = CARTESIAN_POINT ( 'NONE',  ( -12.18289575740000075, 37.87223172089999679, -148.4976681630000144 ) ) ;
#23180 = ORIENTED_EDGE ( 'NONE', *, *, #10306, .F. ) ;
#23181 = CARTESIAN_POINT ( 'NONE',  ( -22.03835531321502117, 36.10604702353144546, -148.4978763513408921 ) ) ;
#23182 = CARTESIAN_POINT ( 'NONE',  ( 31.50000000000000000, 40.03620104870000063, -136.0552959530000123 ) ) ;
#23183 = EDGE_LOOP ( 'NONE', ( #18741, #16979, #1534, #10419 ) ) ;
#23184 = DIRECTION ( 'NONE',  ( 1.000000000000000000, 0.000000000000000000, 0.000000000000000000 ) ) ;
#23185 = AXIS2_PLACEMENT_3D ( 'NONE', #12359, #10344, #19280 ) ;
#23186 = SHAPE_REPRESENTATION ( 'Deadbolt', ( #5025 ), #5047 ) ;
#23187 = AXIS2_PLACEMENT_3D ( 'NONE', #21118, #1261, #11690 ) ;
#23188 = EDGE_CURVE ( 'NONE', #17671, #16792, #14981, .T. ) ;
#23189 = VERTEX_POINT ( 'NONE', #479 ) ;
#23190 = FACE_OUTER_BOUND ( 'NONE', #2972, .T. ) ;
#23191 = AXIS2_PLACEMENT_3D ( 'NONE', #15581, #15702, #22843 ) ;
#23192 = FACE_OUTER_BOUND ( 'NONE', #20664, .T. ) ;
#23193 = EDGE_LOOP ( 'NONE', ( #12779, #8923, #4693, #14720, #17320, #8681, #17198, #3616, #17012, #15808, #1744 ) ) ;
#23194 = DIRECTION ( 'NONE',  ( 1.000000000000000000, 0.000000000000000000, -2.257453483404482811E-12 ) ) ;
#23195 = ADVANCED_FACE ( 'NONE', ( #7377 ), #3929, .T. ) ;
#23196 = DIRECTION ( 'NONE',  ( 1.000000000000000000, 0.000000000000000000, 0.000000000000000000 ) ) ;
#23197 = ORIENTED_EDGE ( 'NONE', *, *, #22457, .T. ) ;
#23198 = CARTESIAN_POINT ( 'NONE',  ( -32.50000000000000000, -14.50000000000000000, -137.0552959530000123 ) ) ;
#23199 = ORIENTED_EDGE ( 'NONE', *, *, #1503, .T. ) ;
#23200 = VECTOR ( 'NONE', #364, 1000.000000000000000 ) ;
#23201 = CARTESIAN_POINT ( 'NONE',  ( -15.50000000000000000, 47.50000000000000000, -151.0552959529999839 ) ) ;
#23202 = CARTESIAN_POINT ( 'NONE',  ( -21.03694116389999635, 36.94210036639999828, -147.9486865819999935 ) ) ;
#23203 = EDGE_CURVE ( 'NONE', #16847, #21680, #13371, .T. ) ;
#23204 = CARTESIAN_POINT ( 'NONE',  ( -14.23530246729999860, 39.72954597060000026, -140.2988105550000171 ) ) ;
#23205 = CARTESIAN_POINT ( 'NONE',  ( -28.59540039647975718, 38.02976288075254274, -140.4496050658455886 ) ) ;
#23206 = ORIENTED_EDGE ( 'NONE', *, *, #9076, .T. ) ;
#23207 = CARTESIAN_POINT ( 'NONE',  ( -9.072898850179999641, 36.94639249900000522, -148.2684494029999769 ) ) ;
#23208 = ADVANCED_FACE ( 'NONE', ( #2041 ), #11394, .F. ) ;
#23209 = DIRECTION ( 'NONE',  ( -0.9892101392001054760, 0.1465035852930155480, 4.471739159800472250E-12 ) ) ;
#23210 = DIRECTION ( 'NONE',  ( 1.000000000000000000, 0.000000000000000000, -2.257157423930000049E-12 ) ) ;
#23211 = LINE ( 'NONE', #21433, #12214 ) ;
#23212 = CARTESIAN_POINT ( 'NONE',  ( 3.999999999879999546, -5.500000000000000000, -135.2552959529999725 ) ) ;
#23213 = ORIENTED_EDGE ( 'NONE', *, *, #5030, .T. ) ;
#23214 = FILL_AREA_STYLE ('',( #14641 ) ) ;
#23215 = EDGE_CURVE ( 'NONE', #20361, #11545, #16882, .T. ) ;
#23216 = FACE_OUTER_BOUND ( 'NONE', #130, .T. ) ;
#23217 = CARTESIAN_POINT ( 'NONE',  ( 24.75935218339999722, -28.32938697159999819, -146.5552959529999839 ) ) ;
#23218 = EDGE_CURVE ( 'NONE', #3418, #14604, #18675, .T. ) ;
#23219 = CARTESIAN_POINT ( 'NONE',  ( -6.938784185830692230, 37.04974994751732709, -148.5388410750851165 ) ) ;
#23220 = CARTESIAN_POINT ( 'NONE',  ( -9.334216945200001447, -17.19633444960000190, -145.5552959529999839 ) ) ;
#23221 = AXIS2_PLACEMENT_3D ( 'NONE', #17340, #15559, #22696 ) ;
#23222 = DIRECTION ( 'NONE',  ( 2.507771768020000122E-12, -0.000000000000000000, -1.000000000000000000 ) ) ;
#23223 = ADVANCED_FACE ( 'NONE', ( #14636 ), #9608, .F. ) ;
#23224 = ORIENTED_EDGE ( 'NONE', *, *, #2443, .F. ) ;
#23225 = DIRECTION ( 'NONE',  ( -1.000000000000000000, 0.000000000000000000, 2.257171095940000041E-12 ) ) ;
#23226 = EDGE_CURVE ( 'NONE', #19149, #7237, #448, .T. ) ;
#23227 = LINE ( 'NONE', #20980, #6010 ) ;
#23228 = ORIENTED_EDGE ( 'NONE', *, *, #16454, .T. ) ;
#23229 = PLANE ( 'NONE',  #3030 ) ;
#23230 = ORIENTED_EDGE ( 'NONE', *, *, #14028, .F. ) ;
#23231 = DIRECTION ( 'NONE',  ( 0.000000000000000000, 0.000000000000000000, -1.000000000000000000 ) ) ;
#23232 = CARTESIAN_POINT ( 'NONE',  ( 19.13369214879999802, -50.49999999980000354, -136.0552959530000123 ) ) ;
#23233 = DIRECTION ( 'NONE',  ( 4.510774274160000731E-12, -1.321907670990000086E-13, 1.000000000000000000 ) ) ;
#23234 = CARTESIAN_POINT ( 'NONE',  ( 7.232790317618205123, 36.19721093022112512, -141.6876531320059200 ) ) ;
#23235 = ORIENTED_EDGE ( 'NONE', *, *, #15175, .T. ) ;
#23236 = CARTESIAN_POINT ( 'NONE',  ( -10.92854443021380106, 33.70908472083943508, -142.0058283514407833 ) ) ;
#23237 = CIRCLE ( 'NONE', #9911, 15.00000000000000178 ) ;
#23238 = CARTESIAN_POINT ( 'NONE',  ( 0.8488726856734599702, 25.45511797032470369, -150.0552959529999839 ) ) ;
#23239 = AXIS2_PLACEMENT_3D ( 'NONE', #1283, #10404, #21384 ) ;
#23240 = DIRECTION ( 'NONE',  ( 0.2451800884060535979, 0.9694775522152123681, -1.317373699560290683E-12 ) ) ;
#23241 = CARTESIAN_POINT ( 'NONE',  ( 4.579308732397330495, -31.65724429029226883, -136.0552959530103294 ) ) ;
#23242 = ORIENTED_EDGE ( 'NONE', *, *, #1379, .T. ) ;
#23243 = LINE ( 'NONE', #46, #19037 ) ;
#23244 =( LENGTH_UNIT ( ) NAMED_UNIT ( * ) SI_UNIT ( .MILLI., .METRE. ) );
#23245 = ADVANCED_FACE ( 'NONE', ( #943 ), #18896, .F. ) ;
#23246 = ORIENTED_EDGE ( 'NONE', *, *, #3592, .T. ) ;
#23247 = CARTESIAN_POINT ( 'NONE',  ( -6.375405121820262089, 34.81974364058724802, -147.0569159591387631 ) ) ;
#23248 = CARTESIAN_POINT ( 'NONE',  ( 22.42370904790000097, -21.41421288319999761, -143.5552959529999839 ) ) ;
#23249 = DIRECTION ( 'NONE',  ( -1.000000000000000000, 0.000000000000000000, -1.457985068979999943E-12 ) ) ;
#23250 = VERTEX_POINT ( 'NONE', #2607 ) ;
#23251 = FACE_OUTER_BOUND ( 'NONE', #16474, .T. ) ;
#23252 = CARTESIAN_POINT ( 'NONE',  ( -13.86630785130000021, -2.273736754430000208E-12, -136.0552959530000123 ) ) ;
#23253 = AXIS2_PLACEMENT_3D ( 'NONE', #6088, #12867, #4306 ) ;
#23254 = AXIS2_PLACEMENT_3D ( 'NONE', #17414, #11685, #1137 ) ;
#23255 = ORIENTED_EDGE ( 'NONE', *, *, #21706, .F. ) ;
#23256 = VECTOR ( 'NONE', #17505, 1000.000000000000000 ) ;
#23257 = CARTESIAN_POINT ( 'NONE',  ( 25.50000000000000000, 19.50000000000000000, -136.5552959530000123 ) ) ;
#23258 = DIRECTION ( 'NONE',  ( 1.000000000000000000, 0.000000000000000000, -1.527536832333223921E-13 ) ) ;
#23259 = PLANE ( 'NONE',  #23421 ) ;
#23260 = CARTESIAN_POINT ( 'NONE',  ( -12.56920363940050223, 37.00563451942269921, -148.6543378380283684 ) ) ;
#23261 = CARTESIAN_POINT ( 'NONE',  ( 13.68320006080000084, -19.50000000000000000, -143.5552959529999839 ) ) ;
#23262 = CARTESIAN_POINT ( 'NONE',  ( -28.90798551740000022, 37.01360947639999921, -139.5686590450000040 ) ) ;
#23263 = LINE ( 'NONE', #3048, #5581 ) ;
#23264 = CARTESIAN_POINT ( 'NONE',  ( -2.492762039218201497, 42.75242722329147682, -136.0552959530022861 ) ) ;
#23265 = CARTESIAN_POINT ( 'NONE',  ( -12.00000000000000000, -43.00000000000000000, -150.0552959529999839 ) ) ;
#23266 = PRODUCT_DEFINITION_SHAPE ( 'NONE', 'NONE',  #14448 ) ;
#23267 = ORIENTED_EDGE ( 'NONE', *, *, #19971, .F. ) ;
#23268 = CARTESIAN_POINT ( 'NONE',  ( -15.57786843150000067, 37.00666880280000726, -148.5521201120000114 ) ) ;
#23269 = VECTOR ( 'NONE', #8098, 1000.000000000000114 ) ;
#23270 = PRODUCT_DEFINITION_CONTEXT ( 'detailed design', #1438, 'design' ) ;
#23271 = VECTOR ( 'NONE', #14262, 1000.000000000000000 ) ;
#23272 = ORIENTED_EDGE ( 'NONE', *, *, #8750, .T. ) ;
#23273 = ADVANCED_FACE ( 'NONE', ( #16994 ), #22953, .F. ) ;
#23274 = ORIENTED_EDGE ( 'NONE', *, *, #22174, .T. ) ;
#23275 = CARTESIAN_POINT ( 'NONE',  ( -16.27122798455739527, 36.16215725498741307, -148.2498576458012849 ) ) ;
#23276 = CARTESIAN_POINT ( 'NONE',  ( -28.21528208400208726, 34.41375009921395645, -140.3410504852042777 ) ) ;
#23277 = ADVANCED_FACE ( 'NONE', ( #8171 ), #17117, .F. ) ;
#23278 = CARTESIAN_POINT ( 'NONE',  ( 1.357896944629999991, -19.89221232270000073, -147.5552959529999839 ) ) ;
#23279 = CARTESIAN_POINT ( 'NONE',  ( 24.89581725840000104, -26.85672394480000236, -144.0552959529999839 ) ) ;
#23280 = ORIENTED_EDGE ( 'NONE', *, *, #15844, .F. ) ;
#23281 = CARTESIAN_POINT ( 'NONE',  ( 22.50000000000000000, 39.50000000000000000, -136.0552959530000123 ) ) ;
#23282 = CARTESIAN_POINT ( 'NONE',  ( -20.24645939794500293, 34.66320656008903711, -141.1397956616578426 ) ) ;
#23283 = CARTESIAN_POINT ( 'NONE',  ( -11.37826538047574765, 40.43565427802512602, -146.2436245357287703 ) ) ;
#23284 = DIRECTION ( 'NONE',  ( 2.257144641399999941E-12, -4.009147065140000298E-51, 1.000000000000000000 ) ) ;
#23285 = ORIENTED_EDGE ( 'NONE', *, *, #1721, .F. ) ;
#23286 = DIRECTION ( 'NONE',  ( 2.839308199620000013E-14, 3.568879590630000244E-13, 1.000000000000000000 ) ) ;
#23287 =( BOUNDED_CURVE ( )  B_SPLINE_CURVE ( 5, ( #4856, #19377, #19499, #10192, #3193, #3084 ),
 .UNSPECIFIED., .F., .F. ) 
 B_SPLINE_CURVE_WITH_KNOTS ( ( 6, 6 ),
 ( 0.000000000000000000, 1.570796326503991924 ),
 .UNSPECIFIED. ) 
 CURVE ( )  GEOMETRIC_REPRESENTATION_ITEM ( )  RATIONAL_B_SPLINE_CURVE ( ( 1.000000000000000000, 0.6000000000741045891, 0.4000000000741046335, 0.3000000000555784752, 0.2500000000370523612, 0.2500000000000000555 ) ) 
 REPRESENTATION_ITEM ( '' )  );
#23288 = ORIENTED_EDGE ( 'NONE', *, *, #1119, .F. ) ;
#23289 = CARTESIAN_POINT ( 'NONE',  ( 9.533096737499036522, 35.91239492147925461, -141.8042231713539536 ) ) ;
#23290 = CARTESIAN_POINT ( 'NONE',  ( -8.100541861814507527, 36.99062475582145737, -140.7379126119400610 ) ) ;
#23291 = LINE ( 'NONE', #17934, #659 ) ;
#23292 = VERTEX_POINT ( 'NONE', #4857 ) ;
#23293 = LINE ( 'NONE', #15685, #6886 ) ;
#23294 = EDGE_LOOP ( 'NONE', ( #10846, #4548, #20761, #20442 ) ) ;
#23295 = DIRECTION ( 'NONE',  ( -2.602084704489999637E-17, 1.000000000000000000, 0.000000000000000000 ) ) ;
#23296 = FACE_OUTER_BOUND ( 'NONE', #19276, .T. ) ;
#23297 = EDGE_LOOP ( 'NONE', ( #19011, #12972, #10808, #9500 ) ) ;
#23298 = CARTESIAN_POINT ( 'NONE',  ( 25.89900052719454848, -22.34364015992473895, -150.0552959529999839 ) ) ;
#23299 = EDGE_LOOP ( 'NONE', ( #10493, #19775, #15469, #9374 ) ) ;
#23300 = ADVANCED_FACE ( 'NONE', ( #1061 ), #7941, .F. ) ;
#23301 = CARTESIAN_POINT ( 'NONE',  ( -15.80598957920876302, 37.98416398598419619, -148.5052001024989181 ) ) ;
#23302 = CARTESIAN_POINT ( 'NONE',  ( -5.500000000000000000, 44.23441892295282685, -150.0552959529999839 ) ) ;
#23303 = EDGE_CURVE ( 'NONE', #8533, #11281, #15691, .T. ) ;
#23304 = VERTEX_POINT ( 'NONE', #22704 ) ;
#23305 = CARTESIAN_POINT ( 'NONE',  ( 0.000000000000000000, 0.000000000000000000, 0.000000000000000000 ) ) ;
#23306 = EDGE_LOOP ( 'NONE', ( #18648, #21716, #17843, #17887 ) ) ;
#23307 = CARTESIAN_POINT ( 'NONE',  ( -26.64637222122986771, 39.75485585484910445, -140.1771219359338829 ) ) ;
#23308 = CARTESIAN_POINT ( 'NONE',  ( -9.282104535849999394, -16.71402168319999859, -144.5552959529999839 ) ) ;
#23309 = EDGE_LOOP ( 'NONE', ( #13510, #15758, #6494, #5740 ) ) ;
#23310 = CARTESIAN_POINT ( 'NONE',  ( -25.85824191589999899, -1.500000000000000000, -146.3157682190000060 ) ) ;
#23311 = CYLINDRICAL_SURFACE ( 'NONE', #4142, 0.5000000000000004441 ) ;
#23312 = ORIENTED_EDGE ( 'NONE', *, *, #11008, .T. ) ;
#23313 = CARTESIAN_POINT ( 'NONE',  ( -12.76385253890000016, 37.02886902030000016, -147.6186336929999925 ) ) ;
#23314 = AXIS2_PLACEMENT_3D ( 'NONE', #19506, #17950, #16165 ) ;
#23315 = ORIENTED_EDGE ( 'NONE', *, *, #4725, .F. ) ;
#23316 = DIRECTION ( 'NONE',  ( -1.000000000000000000, 0.000000000000000000, 0.000000000000000000 ) ) ;
#23317 = ADVANCED_FACE ( 'NONE', ( #2497 ), #4499, .F. ) ;
#23318 = CARTESIAN_POINT ( 'NONE',  ( 25.00000000000000000, -20.50000000000000000, -136.0552959530000123 ) ) ;
#23319 = APPLICATION_CONTEXT ( 'automotive_design' ) ;
#23320 = CARTESIAN_POINT ( 'NONE',  ( -13.87262227687442540, 40.83548773877500793, -141.9013165816338073 ) ) ;
#23321 = CARTESIAN_POINT ( 'NONE',  ( -28.81387671665254757, 37.02484288695368519, -140.6184821045073647 ) ) ;
#23322 = VERTEX_POINT ( 'NONE', #835 ) ;
#23323 = CARTESIAN_POINT ( 'NONE',  ( 1.924189958851657556, 14.53742485369782322, -136.0552959530043324 ) ) ;
#23324 = DIRECTION ( 'NONE',  ( 0.000000000000000000, -1.000000000000000000, 0.000000000000000000 ) ) ;
#23325 =( BOUNDED_SURFACE ( )  B_SPLINE_SURFACE ( 5, 5, ( 
 ( #3805, #3570, #18082, #11267, #8901, #348 ),
 ( #22124, #7474, #16181, #14629, #9363, #7590 ),
 ( #16300, #235, #9014, #11156, #9257, #10918 ),
 ( #2144, #5, #12602, #7254, #14521, #21787 ),
 ( #5472, #12715, #12831, #19984, #11044, #3684 ),
 ( #14865, #9138, #16636, #16418, #128, #18322 ),
 ( #16528, #14738, #12952, #20229, #3922, #22585 ),
 ( #20681, #13527, #7819, #4493, #2380, #11860 ),
 ( #11385, #9601, #18667, #16875, #4147, #22470 ),
 ( #7933, #5924, #583, #937, #8163, #11732 ),
 ( #13179, #22695, #2725, #700, #471, #6391 ),
 ( #13651, #18889, #15087, #20453, #4375, #15328 ) ),
 .UNSPECIFIED., .F., .F., .F. ) 
 B_SPLINE_SURFACE_WITH_KNOTS ( ( 6, 3, 3, 6 ),
 ( 6, 6 ),
 ( 0.000000000000000000, 4.124045064660000648, 8.344666563069999654, 12.67057240369999960 ),
 ( 0.000000000000000000, 1.570796326683649990 ),
 .UNSPECIFIED. ) 
 GEOMETRIC_REPRESENTATION_ITEM ( )  RATIONAL_B_SPLINE_SURFACE ( (
 ( 1.000000000000000000, 0.6000000000283549628, 0.4000000000283550072, 0.3000000000212664775, 0.2500000000141774925, 0.2500000000000000000),
 ( 1.000000000000000000, 0.6000000000283549628, 0.4000000000283550072, 0.3000000000212664775, 0.2500000000141774925, 0.2500000000000000000),
 ( 1.000000000000000000, 0.6000000000283549628, 0.4000000000283550072, 0.3000000000212664775, 0.2500000000141774925, 0.2500000000000000000),
 ( 1.000000000000000000, 0.6000000000283549628, 0.4000000000283550072, 0.3000000000212664775, 0.2500000000141774925, 0.2500000000000000000),
 ( 1.000000000000000000, 0.6000000000283549628, 0.4000000000283550072, 0.3000000000212664775, 0.2500000000141774925, 0.2500000000000000000),
 ( 1.000000000000000000, 0.6000000000283549628, 0.4000000000283550072, 0.3000000000212664775, 0.2500000000141774925, 0.2500000000000000000),
 ( 1.000000000000000000, 0.6000000000283549628, 0.4000000000283550072, 0.3000000000212664775, 0.2500000000141774925, 0.2500000000000000000),
 ( 1.000000000000000000, 0.6000000000283549628, 0.4000000000283550072, 0.3000000000212664775, 0.2500000000141774925, 0.2500000000000000000),
 ( 1.000000000000000000, 0.6000000000283549628, 0.4000000000283550072, 0.3000000000212664775, 0.2500000000141774925, 0.2500000000000000000),
 ( 1.000000000000000000, 0.6000000000283549628, 0.4000000000283550072, 0.3000000000212664775, 0.2500000000141774925, 0.2500000000000000000),
 ( 1.000000000000000000, 0.6000000000283549628, 0.4000000000283550072, 0.3000000000212664775, 0.2500000000141774925, 0.2500000000000000000),
 ( 1.000000000000000000, 0.6000000000283549628, 0.4000000000283550072, 0.3000000000212664775, 0.2500000000141774925, 0.2500000000000000000) ) ) 
 REPRESENTATION_ITEM ( '' )  SURFACE ( )  );
#23326 = DIRECTION ( 'NONE',  ( 1.000000000000000000, 0.000000000000000000, 0.000000000000000000 ) ) ;
#23327 = CARTESIAN_POINT ( 'NONE',  ( -29.13601448249999848, 36.98639052360000079, -140.5419328609999923 ) ) ;
#23328 = DIRECTION ( 'NONE',  ( 0.000000000000000000, 0.000000000000000000, 1.000000000000000000 ) ) ;
#23329 = DIRECTION ( 'NONE',  ( 0.000000000000000000, -1.000000000000000000, 3.568879590630000244E-13 ) ) ;
#23330 = EDGE_CURVE ( 'NONE', #1998, #17682, #1193, .T. ) ;
#23331 = VERTEX_POINT ( 'NONE', #19020 ) ;
#23332 =( LENGTH_UNIT ( ) NAMED_UNIT ( * ) SI_UNIT ( .MILLI., .METRE. ) );
#23333 = FACE_OUTER_BOUND ( 'NONE', #14545, .T. ) ;
#23334 = FACE_OUTER_BOUND ( 'NONE', #4387, .T. ) ;
#23335 = CARTESIAN_POINT ( 'NONE',  ( -5.847812726100290348, 39.76587201757381962, -147.8755786061779816 ) ) ;
#23336 = CARTESIAN_POINT ( 'NONE',  ( -7.806459626920000616, 32.86659014889999497, -143.7778124400000195 ) ) ;
#23337 = LINE ( 'NONE', #14291, #6452 ) ;
#23338 = ORIENTED_EDGE ( 'NONE', *, *, #8983, .F. ) ;
#23339 = VECTOR ( 'NONE', #10464, 1000.000000000000000 ) ;
#23340 = PLANE ( 'NONE',  #21242 ) ;
#23341 = EDGE_CURVE ( 'NONE', #20820, #4706, #8057, .T. ) ;
#23342 = DIRECTION ( 'NONE',  ( 1.000000000000000000, 0.000000000000000000, 0.000000000000000000 ) ) ;
#23343 = VERTEX_POINT ( 'NONE', #19247 ) ;
#23344 = FACE_OUTER_BOUND ( 'NONE', #16166, .T. ) ;
#23345 = VERTEX_POINT ( 'NONE', #17468 ) ;
#23346 = FACE_OUTER_BOUND ( 'NONE', #143, .T. ) ;
#23347 = EDGE_CURVE ( 'NONE', #6863, #5196, #19137, .T. ) ;
#23348 = CARTESIAN_POINT ( 'NONE',  ( -29.04405754842699849, 38.20917013907699555, -139.5702141476339762 ) ) ;
#23349 = EDGE_CURVE ( 'NONE', #21958, #2149, #6170, .T. ) ;
#23350 = CARTESIAN_POINT ( 'NONE',  ( -34.50000000000000000, -64.50000000000000000, -144.0552959529999839 ) ) ;
#23351 = CARTESIAN_POINT ( 'NONE',  ( 7.838941837282176195, 38.34734725831290802, -141.9492515416635001 ) ) ;
#23352 = ORIENTED_EDGE ( 'NONE', *, *, #11263, .T. ) ;
#23353 = CARTESIAN_POINT ( 'NONE',  ( -11.59475511509054257, 36.93163239414370480, -139.6817994054218559 ) ) ;
#23354 = DIRECTION ( 'NONE',  ( 1.211690350419999855E-27, 2.765629237170000203E-27, -1.000000000000000000 ) ) ;
#23355 = EDGE_CURVE ( 'NONE', #15840, #9450, #18920, .T. ) ;
#23356 = DIRECTION ( 'NONE',  ( -0.7071067811865475727, -0.7071067811865475727, 1.595020412044807153E-12 ) ) ;
#23357 = CYLINDRICAL_SURFACE ( 'NONE', #8778, 0.7499999999999997780 ) ;
#23358 = AXIS2_PLACEMENT_3D ( 'NONE', #9996, #17389, #21089 ) ;
#23359 = ADVANCED_FACE ( 'NONE', ( #4977 ), #23413, .T. ) ;
#23360 = ORIENTED_EDGE ( 'NONE', *, *, #19440, .F. ) ;
#23361 = FACE_OUTER_BOUND ( 'NONE', #17105, .T. ) ;
#23362 = PRESENTATION_STYLE_ASSIGNMENT (( #5264 ) ) ;
#23363 = ORIENTED_EDGE ( 'NONE', *, *, #10626, .T. ) ;
#23364 = DIRECTION ( 'NONE',  ( -4.537894428437109619E-14, 0.000000000000000000, 1.000000000000000000 ) ) ;
#23365 = DIRECTION ( 'NONE',  ( -2.507771768019999718E-12, -1.592654864069999939E-17, 1.000000000000000000 ) ) ;
#23366 = CARTESIAN_POINT ( 'NONE',  ( 12.18320006080000084, -21.50000000000000000, -148.5552959529999839 ) ) ;
#23367 = ORIENTED_EDGE ( 'NONE', *, *, #16575, .F. ) ;
#23368 = CARTESIAN_POINT ( 'NONE',  ( 6.500000000140000012, 28.50000000000000000, -146.5552959529999839 ) ) ;
#23369 = LINE ( 'NONE', #19919, #1547 ) ;
#23370 = VERTEX_POINT ( 'NONE', #17945 ) ;
#23371 = CARTESIAN_POINT ( 'NONE',  ( -17.27864984460000031, 40.23496799359999443, -142.1532139960000052 ) ) ;
#23372 = DIRECTION ( 'NONE',  ( 0.000000000000000000, -1.000000000000000000, 0.000000000000000000 ) ) ;
#23374 = AXIS2_PLACEMENT_3D ( 'NONE', #3214, #10445, #17369 ) ;
#23373 = LINE ( 'NONE', #14678, #632 ) ;
#23375 = CARTESIAN_POINT ( 'NONE',  ( 3.000000000000000000, -3.500000000000000000, -140.0552959529999839 ) ) ;
#23376 = LINE ( 'NONE', #23144, #11589 ) ;
#23377 = EDGE_CURVE ( 'NONE', #14581, #21645, #16277, .T. ) ;
#23378 = CARTESIAN_POINT ( 'NONE',  ( -16.81794493339999619, 37.02435727940000731, -140.5111119820000170 ) ) ;
#23379 = PRODUCT_CONTEXT ( 'NONE', #18899, 'mechanical' ) ;
#23380 = FACE_OUTER_BOUND ( 'NONE', #22708, .T. ) ;
#23381 = CARTESIAN_POINT ( 'NONE',  ( 24.41610067590000099, -29.22497285029999858, -143.5552959529999839 ) ) ;
#23382 = CARTESIAN_POINT ( 'NONE',  ( -12.00000000000000000, -43.00000000000000000, -140.0552959529999839 ) ) ;
#23383 = EDGE_LOOP ( 'NONE', ( #8998, #7915, #14713, #18128, #15784 ) ) ;
#23384 = ORIENTED_EDGE ( 'NONE', *, *, #531, .T. ) ;
#23385 = CARTESIAN_POINT ( 'NONE',  ( 0.000000000000000000, 0.000000000000000000, 0.000000000000000000 ) ) ;
#23386 = ORIENTED_EDGE ( 'NONE', *, *, #391, .T. ) ;
#23387 = VECTOR ( 'NONE', #1355, 1000.000000000000000 ) ;
#23388 = CARTESIAN_POINT ( 'NONE',  ( -15.68268784160000173, 36.02211616019999951, -148.5535485649999998 ) ) ;
#23389 = CARTESIAN_POINT ( 'NONE',  ( -32.50000000000000000, -50.50000000000000000, -136.0552959530000123 ) ) ;
#23390 = CARTESIAN_POINT ( 'NONE',  ( -13.86630785140000022, -51.50000000000000000, -136.5552959530000123 ) ) ;
#23391 = VECTOR ( 'NONE', #14680, 1000.000000000000000 ) ;
#23392 = CARTESIAN_POINT ( 'NONE',  ( 8.915777720213307944, 27.61753626548637897, -136.0552959530201065 ) ) ;
#23393 = ORIENTED_EDGE ( 'NONE', *, *, #12130, .F. ) ;
#23394 = DIRECTION ( 'NONE',  ( 7.105427352510001232E-15, -1.000000000000000000, -1.603797727360000188E-26 ) ) ;
#23395 = CARTESIAN_POINT ( 'NONE',  ( -20.44384907338949375, 36.15213303015924851, -140.4838640016932629 ) ) ;
#23396 = CARTESIAN_POINT ( 'NONE',  ( -11.97376781498133447, 40.01783495556804837, -145.9099724590802225 ) ) ;
#23397 = CARTESIAN_POINT ( 'NONE',  ( -32.50000000000000000, 1.000000000000000000, -149.5552959529999839 ) ) ;
#23398 = EDGE_LOOP ( 'NONE', ( #6425, #16050, #14638, #5023 ) ) ;
#23399 = PLANE ( 'NONE',  #3829 ) ;
#23400 = ORIENTED_EDGE ( 'NONE', *, *, #15785, .F. ) ;
#23401 = CARTESIAN_POINT ( 'NONE',  ( 9.069815628852895273, 35.61242929765868581, -141.9757830863595700 ) ) ;
#23402 = EDGE_CURVE ( 'NONE', #21143, #6545, #6750, .T. ) ;
#23403 = DIRECTION ( 'NONE',  ( 1.000000000000000000, 0.000000000000000000, 0.000000000000000000 ) ) ;
#23404 = VECTOR ( 'NONE', #9368, 1000.000000000000000 ) ;
#23405 = CARTESIAN_POINT ( 'NONE',  ( -35.07300000000000040, 14.00000000000000000, -144.5552959529999839 ) ) ;
#23406 = AXIS2_PLACEMENT_3D ( 'NONE', #16000, #1150, #22912 ) ;
#23407 = EDGE_LOOP ( 'NONE', ( #17804, #17200, #2341, #22925 ) ) ;
#23408 = DIRECTION ( 'NONE',  ( 2.257157423930000049E-12, 0.000000000000000000, 1.000000000000000000 ) ) ;
#23409 = EDGE_LOOP ( 'NONE', ( #5068, #11629, #453, #11356 ) ) ;
#23410 = CARTESIAN_POINT ( 'NONE',  ( -13.86630785130000021, 51.50000000000000000, -136.0552959530000123 ) ) ;
#23411 = CARTESIAN_POINT ( 'NONE',  ( -12.50000000000000000, 45.50000000000000000, -150.0552959529999839 ) ) ;
#23412 = ORIENTED_EDGE ( 'NONE', *, *, #68, .T. ) ;
#23413 = PLANE ( 'NONE',  #22883 ) ;
#23414 = VERTEX_POINT ( 'NONE', #5330 ) ;
#23415 = CARTESIAN_POINT ( 'NONE',  ( 3.000000000010000001, -3.500000000000000000, -137.0552959530000123 ) ) ;
#23416 = CARTESIAN_POINT ( 'NONE',  ( -9.350215169903842494, -17.08637274644199522, -147.5552959529998134 ) ) ;
#23417 = ORIENTED_EDGE ( 'NONE', *, *, #23349, .F. ) ;
#23418 = DIRECTION ( 'NONE',  ( 0.000000000000000000, 0.000000000000000000, 1.000000000000000000 ) ) ;
#23419 = ORIENTED_EDGE ( 'NONE', *, *, #14913, .F. ) ;
#23420 = LINE ( 'NONE', #5210, #6450 ) ;
#23421 = AXIS2_PLACEMENT_3D ( 'NONE', #14096, #13858, #6950 ) ;
#23422 = CARTESIAN_POINT ( 'NONE',  ( 31.50000000000000000, 0.000000000000000000, -149.5552959529999839 ) ) ;
#23423 = ORIENTED_EDGE ( 'NONE', *, *, #3889, .T. ) ;
#23424 = VECTOR ( 'NONE', #1947, 1000.000000000000000 ) ;
#23425 = DIRECTION ( 'NONE',  ( 1.000000000000000000, 0.000000000000000000, 0.000000000000000000 ) ) ;
#23426 = CARTESIAN_POINT ( 'NONE',  ( -10.36675979729999852, 34.52853970540000006, -140.3392284379999921 ) ) ;
#23427 = CARTESIAN_POINT ( 'NONE',  ( 14.50000000010000001, 37.00000000000000000, -144.0552959529999839 ) ) ;
#23428 = VERTEX_POINT ( 'NONE', #14497 ) ;
#23429 = DIRECTION ( 'NONE',  ( 2.257242012349999735E-12, 0.000000000000000000, 1.000000000000000000 ) ) ;
#23430 = ADVANCED_FACE ( 'NONE', ( #12225, #1773 ), #14139, .F. ) ;
#23431 = EDGE_CURVE ( 'NONE', #8533, #17860, #7231, .T. ) ;
#23432 = ORIENTED_EDGE ( 'NONE', *, *, #22446, .T. ) ;
#23433 = CARTESIAN_POINT ( 'NONE',  ( -30.50000000000000000, 26.50000000000000000, -149.0552959529999839 ) ) ;
#23434 = DIRECTION ( 'NONE',  ( 0.000000000000000000, 0.7071067811870332953, 0.7071067811860618502 ) ) ;
#23435 = DIRECTION ( 'NONE',  ( -1.000000000000000000, 0.000000000000000000, -2.507771768020000122E-12 ) ) ;
#23436 = DIRECTION ( 'NONE',  ( 0.000000000000000000, 1.000000000000000000, 0.000000000000000000 ) ) ;
#23437 = VECTOR ( 'NONE', #10860, 1000.000000000000000 ) ;
#23438 = VERTEX_POINT ( 'NONE', #6992 ) ;
#23439 = CARTESIAN_POINT ( 'NONE',  ( -7.149448239889999890, -25.45628515800000002, -146.0552959529999839 ) ) ;
#23440 = DIRECTION ( 'NONE',  ( 1.000000000000000000, 0.000000000000000000, 2.516505522483685870E-12 ) ) ;
#23441 = DIRECTION ( 'NONE',  ( 1.000000000000000000, 0.000000000000000000, -4.430318231639999944E-12 ) ) ;
#23442 = CARTESIAN_POINT ( 'NONE',  ( -28.33971964075504957, 37.08144121879503530, -140.0461821376672162 ) ) ;
#23443 = CARTESIAN_POINT ( 'NONE',  ( 17.45728951470000112, -20.98759093920000041, -147.5552959529999839 ) ) ;
#23444 = DIRECTION ( 'NONE',  ( 1.000000000000000000, -5.094701932209999624E-24, 0.000000000000000000 ) ) ;
#23445 = ORIENTED_EDGE ( 'NONE', *, *, #1906, .T. ) ;
#23446 = DIRECTION ( 'NONE',  ( 0.000000000000000000, 0.000000000000000000, 1.000000000000000000 ) ) ;
#23447 = CARTESIAN_POINT ( 'NONE',  ( -14.80113973143733119, -41.50000000000002132, -136.0552959529666168 ) ) ;
#23448 = CARTESIAN_POINT ( 'NONE',  ( -13.37265858230000148, 32.83955069500000690, -141.7941727500000013 ) ) ;
#23449 = DIRECTION ( 'NONE',  ( 1.000000000000000000, 0.000000000000000000, 0.000000000000000000 ) ) ;
#23450 = LINE ( 'NONE', #3699, #1716 ) ;
#23451 = VECTOR ( 'NONE', #3741, 1000.000000000000000 ) ;
#23452 = ORIENTED_EDGE ( 'NONE', *, *, #6482, .T. ) ;
#23453 = CARTESIAN_POINT ( 'NONE',  ( -26.59168384020000175, 38.48554521319999822, -140.5676127940000129 ) ) ;
#23454 =( GEOMETRIC_REPRESENTATION_CONTEXT ( 3 ) GLOBAL_UNCERTAINTY_ASSIGNED_CONTEXT ( ( #14463 ) ) GLOBAL_UNIT_ASSIGNED_CONTEXT ( ( #22385, #2299, #18354 ) ) REPRESENTATION_CONTEXT ( 'NONE', 'WORKASPACE' ) );
#23455 = FACE_BOUND ( 'NONE', #15671, .T. ) ;
#23456 = VERTEX_POINT ( 'NONE', #14013 ) ;
#23457 = EDGE_CURVE ( 'NONE', #10188, #9539, #17704, .T. ) ;
#23458 = DIRECTION ( 'NONE',  ( 0.000000000000000000, -1.000000000000000000, -1.592654864069999939E-17 ) ) ;
#23459 = ORIENTED_EDGE ( 'NONE', *, *, #2941, .T. ) ;
#23460 =( BOUNDED_SURFACE ( )  B_SPLINE_SURFACE ( 5, 5, ( 
 ( #18466, #20377, #16912, #2179, #20493, #511 ),
 ( #7745, #5964, #14783, #17025, #18359, #15130 ),
 ( #22392, #4193, #13218, #6090, #11306, #13342 ),
 ( #9402, #18582, #4309, #20614, #2304, #22513 ),
 ( #4069, #11539, #9749, #14902, #6205, #9530 ),
 ( #22049, #2071, #745, #12993, #7631, #22161 ),
 ( #5846, #13103, #14052, #1099, #8329, #12138 ),
 ( #13567, #8559, #10350, #15719, #17149, #15478 ),
 ( #869, #4536, #15831, #22623, #1334, #2644 ),
 ( #8452, #19285, #3118, #4890, #23095, #10233 ),
 ( #19168, #11776, #13696, #12020, #20841, #13822 ),
 ( #6786, #21320, #9875, #11653, #17502, #22982 ) ),
 .UNSPECIFIED., .F., .F., .F. ) 
 B_SPLINE_SURFACE_WITH_KNOTS ( ( 6, 3, 3, 6 ),
 ( 6, 6 ),
 ( 0.000000000000000000, 4.358589029760000066, 8.533830367689999363, 12.54112731390000057 ),
 ( 0.000000000000000000, 1.570796326769924978 ),
 .UNSPECIFIED. ) 
 GEOMETRIC_REPRESENTATION_ITEM ( )  RATIONAL_B_SPLINE_SURFACE ( (
 ( 1.000000000000000000, 0.6000000000063859806, 0.4000000000063860250, 0.3000000000047894910, 0.2500000000031930014, 0.2500000000000000000),
 ( 1.000000000000000000, 0.6000000000063859806, 0.4000000000063860250, 0.3000000000047894910, 0.2500000000031930014, 0.2500000000000000000),
 ( 1.000000000000000000, 0.6000000000063859806, 0.4000000000063860250, 0.3000000000047894910, 0.2500000000031930014, 0.2500000000000000000),
 ( 1.000000000000000000, 0.6000000000063859806, 0.4000000000063860250, 0.3000000000047894910, 0.2500000000031930014, 0.2500000000000000000),
 ( 1.000000000000000000, 0.6000000000063859806, 0.4000000000063860250, 0.3000000000047894910, 0.2500000000031930014, 0.2500000000000000000),
 ( 1.000000000000000000, 0.6000000000063859806, 0.4000000000063860250, 0.3000000000047894910, 0.2500000000031930014, 0.2500000000000000000),
 ( 1.000000000000000000, 0.6000000000063859806, 0.4000000000063860250, 0.3000000000047894910, 0.2500000000031930014, 0.2500000000000000000),
 ( 1.000000000000000000, 0.6000000000063859806, 0.4000000000063860250, 0.3000000000047894910, 0.2500000000031930014, 0.2500000000000000000),
 ( 1.000000000000000000, 0.6000000000063859806, 0.4000000000063860250, 0.3000000000047894910, 0.2500000000031930014, 0.2500000000000000000),
 ( 1.000000000000000000, 0.6000000000063859806, 0.4000000000063860250, 0.3000000000047894910, 0.2500000000031930014, 0.2500000000000000000),
 ( 1.000000000000000000, 0.6000000000063859806, 0.4000000000063860250, 0.3000000000047894910, 0.2500000000031930014, 0.2500000000000000000),
 ( 1.000000000000000000, 0.6000000000063859806, 0.4000000000063860250, 0.3000000000047894910, 0.2500000000031930014, 0.2500000000000000000) ) ) 
 REPRESENTATION_ITEM ( '' )  SURFACE ( )  );
#23461 = CARTESIAN_POINT ( 'NONE',  ( -24.49703822390000241, 40.50511125069999707, -146.0729279460000214 ) ) ;
#23462 = DIRECTION ( 'NONE',  ( 1.000000000000000000, 0.000000000000000000, 2.504935852220000146E-12 ) ) ;
#23463 = DIRECTION ( 'NONE',  ( -1.000000000000000000, 0.000000000000000000, 0.000000000000000000 ) ) ;
#23464 = CARTESIAN_POINT ( 'NONE',  ( 8.002304315546503233, 38.41542824385604149, -141.9945801900086622 ) ) ;
#23465 = ORIENTED_EDGE ( 'NONE', *, *, #14838, .F. ) ;
#23466 = CARTESIAN_POINT ( 'NONE',  ( -11.38486064677451992, 36.95668670076564410, -140.3965526144922080 ) ) ;
#23467 = CARTESIAN_POINT ( 'NONE',  ( -18.75102069614494837, 32.86990036210830368, -146.6269676767523720 ) ) ;
#23468 = AXIS2_PLACEMENT_3D ( 'NONE', #9981, #9865, #4648 ) ;
#23469 = CARTESIAN_POINT ( 'NONE',  ( -9.701308260419525098, 37.75684802965571407, -147.4734421784763754 ) ) ;
#23470 = DIRECTION ( 'NONE',  ( 2.602084747549999882E-17, -1.000000000000000000, -5.873289694040000105E-29 ) ) ;
#23471 = ADVANCED_FACE ( 'NONE', ( #3085 ), #17594, .T. ) ;
#23472 = ORIENTED_EDGE ( 'NONE', *, *, #8469, .F. ) ;
#23473 = DIRECTION ( 'NONE',  ( 4.430318231636070029E-12, -6.100259101526210011E-13, 1.000000000000000000 ) ) ;
#23474 = ORIENTED_EDGE ( 'NONE', *, *, #3682, .T. ) ;
#23475 = DIRECTION ( 'NONE',  ( 3.994014902950000436E-29, -1.000000000000000000, 4.148443855749999753E-27 ) ) ;
#23476 = DIRECTION ( 'NONE',  ( 1.000000000000000000, 0.000000000000000000, -4.430318231639999944E-12 ) ) ;
#23477 = DIRECTION ( 'NONE',  ( -0.6459422414661292189, 0.7633862853691524286, 0.000000000000000000 ) ) ;
#23478 = EDGE_CURVE ( 'NONE', #23072, #4899, #22506, .T. ) ;
#23479 = EDGE_LOOP ( 'NONE', ( #11022, #8340, #22954, #10775 ) ) ;
#23480 = CARTESIAN_POINT ( 'NONE',  ( -4.499999999949999996, 31.50000000000000000, -150.0552959529999839 ) ) ;
#23481 = FACE_OUTER_BOUND ( 'NONE', #18426, .T. ) ;
#23482 = EDGE_CURVE ( 'NONE', #16530, #4528, #4422, .T. ) ;
#23483 = ORIENTED_EDGE ( 'NONE', *, *, #18715, .T. ) ;
#23484 = DIRECTION ( 'NONE',  ( 0.000000000000000000, 7.657380550038349542E-13, -1.000000000000000000 ) ) ;
#23485 = EDGE_CURVE ( 'NONE', #12734, #9016, #18331, .T. ) ;
#23486 = EDGE_CURVE ( 'NONE', #5559, #1590, #3305, .T. ) ;
#23487 = CARTESIAN_POINT ( 'NONE',  ( -32.50000000000000000, 0.9999999999959999775, -144.0552959529999839 ) ) ;
#23488 = VECTOR ( 'NONE', #11128, 1000.000000000000000 ) ;
#23489 = LINE ( 'NONE', #5408, #9720 ) ;
#23490 = DIRECTION ( 'NONE',  ( 1.190078432789999897E-50, 1.000000000000000000, 0.000000000000000000 ) ) ;
#23491 = DIRECTION ( 'NONE',  ( 0.000000000000000000, -1.000000000000000000, 0.000000000000000000 ) ) ;
#23492 = DIRECTION ( 'NONE',  ( -0.04169410462551791791, 0.9991304227374304681, -3.553937932771528679E-13 ) ) ;
#23493 = DIRECTION ( 'NONE',  ( -1.000000000000000000, 0.000000000000000000, 0.000000000000000000 ) ) ;
#23494 = DIRECTION ( 'NONE',  ( 1.000000000000000000, 0.000000000000000000, -2.259303855112193560E-12 ) ) ;
#23495 = CARTESIAN_POINT ( 'NONE',  ( 20.35976161480000002, -31.74228192520000391, -146.5552959529999839 ) ) ;
#23496 = EDGE_CURVE ( 'NONE', #18574, #9140, #21640, .T. ) ;
#23497 = ORIENTED_EDGE ( 'NONE', *, *, #11837, .T. ) ;
#23498 = UNCERTAINTY_MEASURE_WITH_UNIT (LENGTH_MEASURE( 1.000000000000000082E-05 ), #19987, 'distance_accuracy_value', 'NONE');
#23499 = ADVANCED_FACE ( 'NONE', ( #10776 ), #106, .T. ) ;
#23501 = VERTEX_POINT ( 'NONE', #21874 ) ;
#23500 = AXIS2_PLACEMENT_3D ( 'NONE', #12147, #19541, #15730 ) ;
#23502 =( LENGTH_UNIT ( ) NAMED_UNIT ( * ) SI_UNIT ( .MILLI., .METRE. ) );
#23503 = VECTOR ( 'NONE', #15602, 1000.000000000000114 ) ;
#23504 = EDGE_LOOP ( 'NONE', ( #21529, #16688, #9852, #14210 ) ) ;
#23505 = DIRECTION ( 'NONE',  ( -0.9938526945756316344, 0.1107105301439589573, 6.178155812097707047E-14 ) ) ;
#23506 = CARTESIAN_POINT ( 'NONE',  ( 31.00000000000000000, -39.80430157320000006, -149.5552959529999839 ) ) ;
#23507 = EDGE_LOOP ( 'NONE', ( #14419, #12215, #11983, #2451 ) ) ;
#23508 = DIRECTION ( 'NONE',  ( 1.000000000000000000, 0.000000000000000000, 0.000000000000000000 ) ) ;
#23509 = ADVANCED_FACE ( 'NONE', ( #22099 ), #11619, .F. ) ;
#23510 = ORIENTED_EDGE ( 'NONE', *, *, #1837, .T. ) ;
#23511 = CIRCLE ( 'NONE', #13237, 4.000000000000001776 ) ;
#23512 = PLANE ( 'NONE',  #12129 ) ;
#23513 = CARTESIAN_POINT ( 'NONE',  ( 17.21087225569999646, -22.66053313549999970, -144.5552959529999839 ) ) ;
#23514 = EDGE_CURVE ( 'NONE', #76, #11004, #17199, .T. ) ;
#23515 = CARTESIAN_POINT ( 'NONE',  ( -11.40579923052419176, 40.54540395906296624, -144.5952108064055608 ) ) ;
#23516 = LINE ( 'NONE', #16380, #17902 ) ;
#23517 = VERTEX_POINT ( 'NONE', #13626 ) ;
#23518 = FACE_BOUND ( 'NONE', #12030, .T. ) ;
#23519 = EDGE_CURVE ( 'NONE', #18727, #6756, #11952, .T. ) ;
#23520 = ORIENTED_EDGE ( 'NONE', *, *, #19262, .F. ) ;
#23521 = CARTESIAN_POINT ( 'NONE',  ( 9.428880901062701270, 35.82197050348334955, -141.8499009806686786 ) ) ;
#23522 = VECTOR ( 'NONE', #4486, 1000.000000000000000 ) ;
#23523 = DIRECTION ( 'NONE',  ( 2.257144641404620116E-12, 2.777754792983395132E-24, 1.000000000000000000 ) ) ;
#23524 = CARTESIAN_POINT ( 'NONE',  ( -34.50000000000000000, 66.54114892279999083, -145.8104610769999852 ) ) ;
#23525 = VERTEX_POINT ( 'NONE', #2928 ) ;
#23526 = VECTOR ( 'NONE', #11992, 1000.000000000000000 ) ;
#23527 = VECTOR ( 'NONE', #21065, 1000.000000000000227 ) ;
#23528 = CARTESIAN_POINT ( 'NONE',  ( -14.47770030809999930, -34.50000000000000000, -150.0552959529999839 ) ) ;
#23529 = ORIENTED_EDGE ( 'NONE', *, *, #22147, .F. ) ;
#23530 = FACE_OUTER_BOUND ( 'NONE', #17765, .T. ) ;
#23531 = DIRECTION ( 'NONE',  ( -1.000000000000000000, -2.602084704489999637E-17, 1.701177084830000066E-20 ) ) ;
#23532 = ORIENTED_EDGE ( 'NONE', *, *, #18385, .T. ) ;
#23533 = CARTESIAN_POINT ( 'NONE',  ( -13.86630785140000022, -51.50000000000000000, -137.0552959530000123 ) ) ;
#23534 = ORIENTED_EDGE ( 'NONE', *, *, #16809, .F. ) ;
#23535 = CARTESIAN_POINT ( 'NONE',  ( -22.25292207123187893, 34.30819563794508298, -147.7538981111728731 ) ) ;
#23536 = CARTESIAN_POINT ( 'NONE',  ( -5.449075813509844934, 45.02080533206359547, -136.0552959529877342 ) ) ;
#23537 = ORIENTED_EDGE ( 'NONE', *, *, #9279, .T. ) ;
#23538 = VECTOR ( 'NONE', #9597, 1000.000000000000000 ) ;
#23539 = EDGE_CURVE ( 'NONE', #8887, #2628, #11459, .T. ) ;
#23540 = CARTESIAN_POINT ( 'NONE',  ( -29.13601448249999848, 36.98639052360000079, -140.5419328609999923 ) ) ;
#23541 = NEXT_ASSEMBLY_USAGE_OCCURRENCE ( 'NAUO1', ' ', ' ', #4990, #3542, $ ) ;
#23542 = NEXT_ASSEMBLY_USAGE_OCCURRENCE ( 'NAUO2', ' ', ' ', #4990, #1805, $ ) ;
#23543 = NEXT_ASSEMBLY_USAGE_OCCURRENCE ( 'NAUO3', ' ', ' ', #4990, #19394, $ ) ;
#23544 = NEXT_ASSEMBLY_USAGE_OCCURRENCE ( 'NAUO4', ' ', ' ', #4990, #11950, $ ) ;
#23545 = NEXT_ASSEMBLY_USAGE_OCCURRENCE ( 'NAUO5', ' ', ' ', #4990, #10930, $ ) ;
#23546 = NEXT_ASSEMBLY_USAGE_OCCURRENCE ( 'NAUO6', ' ', ' ', #4990, #6720, $ ) ;
#23547 = NEXT_ASSEMBLY_USAGE_OCCURRENCE ( 'NAUO7', ' ', ' ', #4990, #20119, $ ) ;
#23548 = NEXT_ASSEMBLY_USAGE_OCCURRENCE ( 'NAUO8', ' ', ' ', #4990, #16194, $ ) ;
#23549 = NEXT_ASSEMBLY_USAGE_OCCURRENCE ( 'NAUO9', ' ', ' ', #4990, #14448, $ ) ;
#23550 = NEXT_ASSEMBLY_USAGE_OCCURRENCE ( 'NAUO10', ' ', ' ', #4990, #8754, $ ) ;
#23551 = NEXT_ASSEMBLY_USAGE_OCCURRENCE ( 'NAUO11', ' ', ' ', #4990, #10209, $ ) ;
#23552 = NEXT_ASSEMBLY_USAGE_OCCURRENCE ( 'NAUO12', ' ', ' ', #4990, #1074, $ ) ;
#23553 = NEXT_ASSEMBLY_USAGE_OCCURRENCE ( 'NAUO13', ' ', ' ', #4990, #781, $ ) ;
#23554 = NEXT_ASSEMBLY_USAGE_OCCURRENCE ( 'NAUO14', ' ', ' ', #4990, #14448, $ ) ;
ENDSEC;
END-ISO-10303-21;
